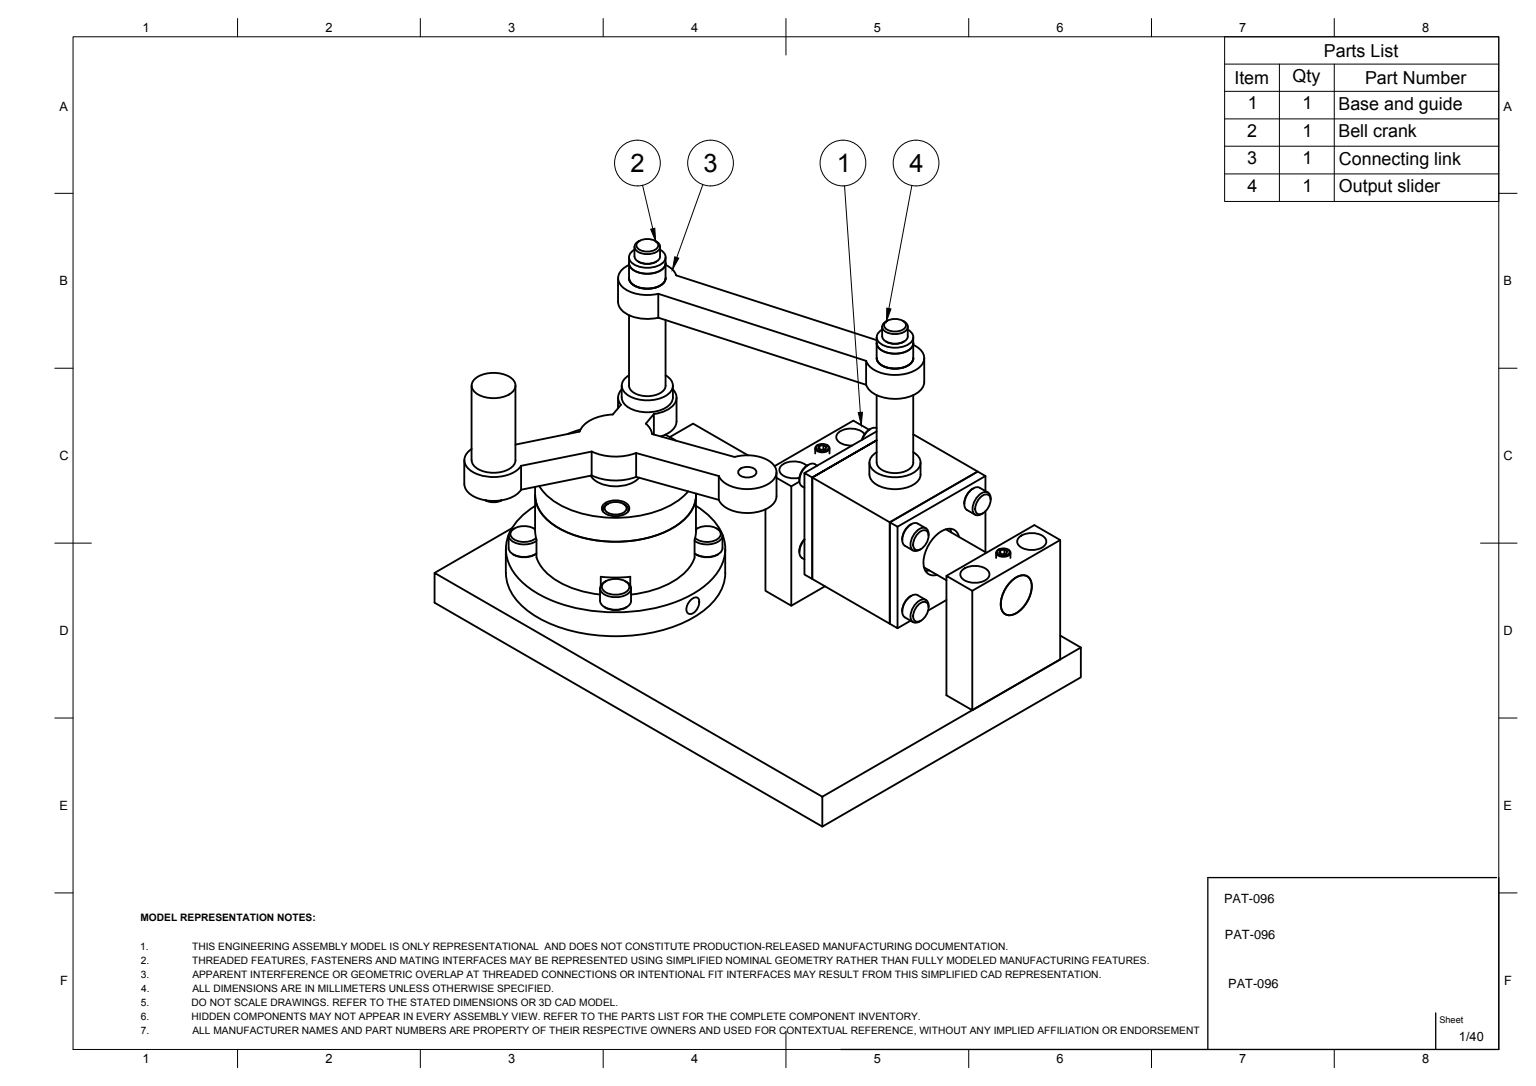
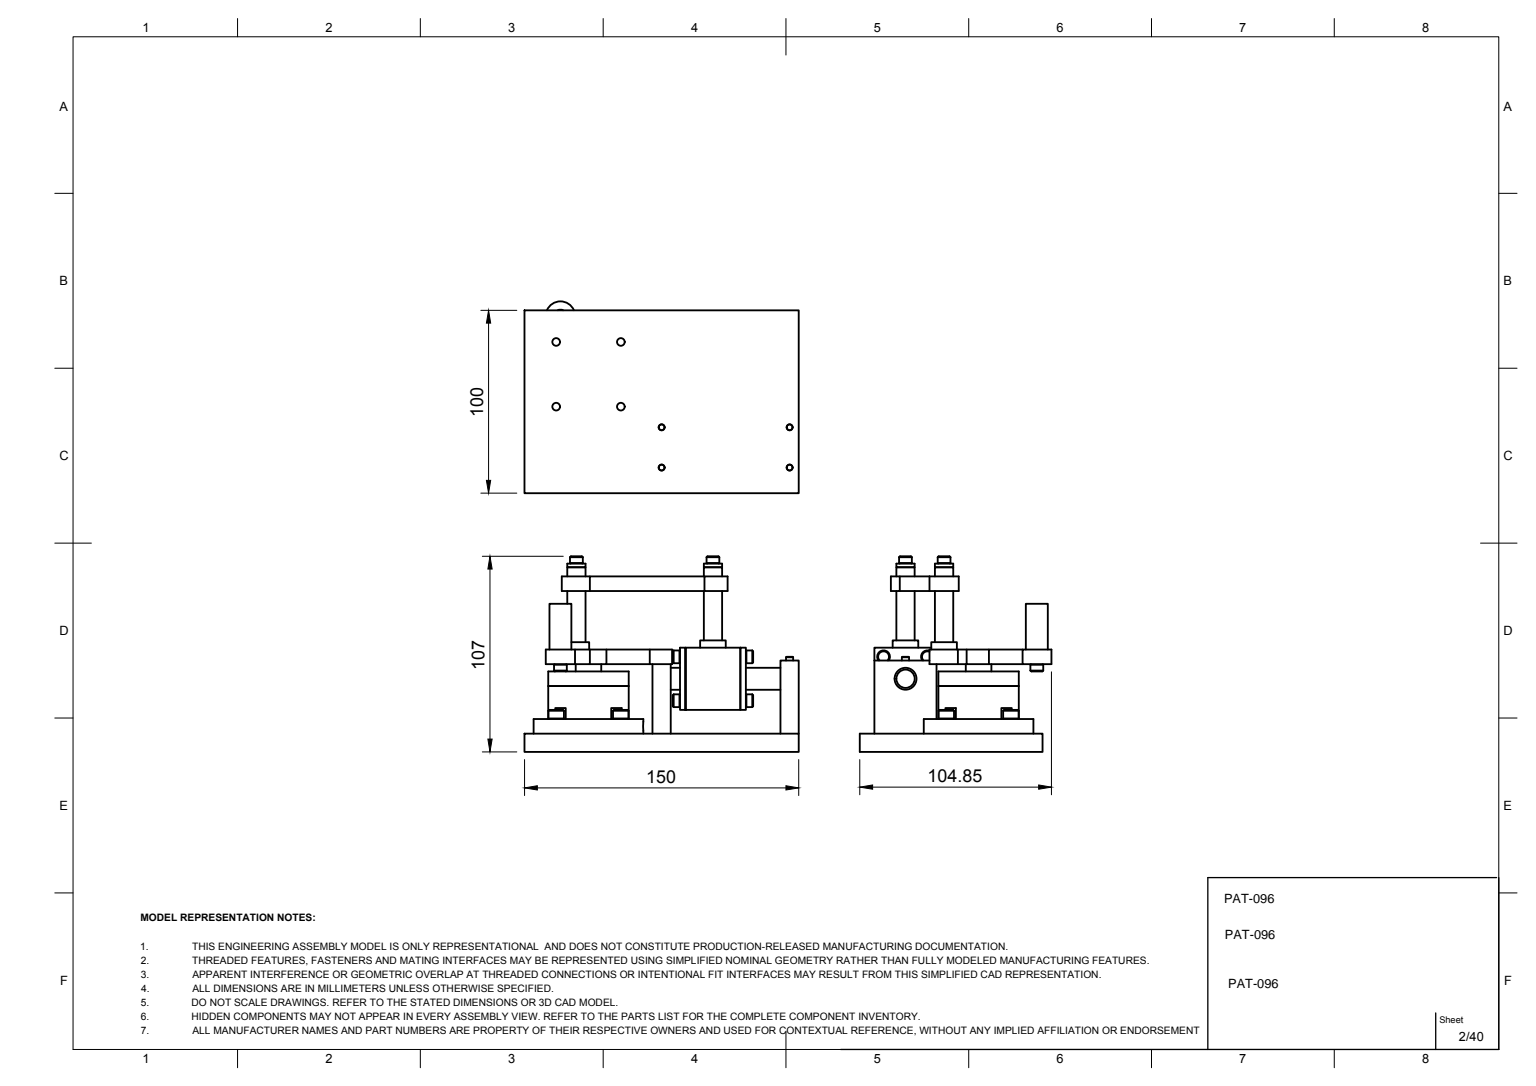
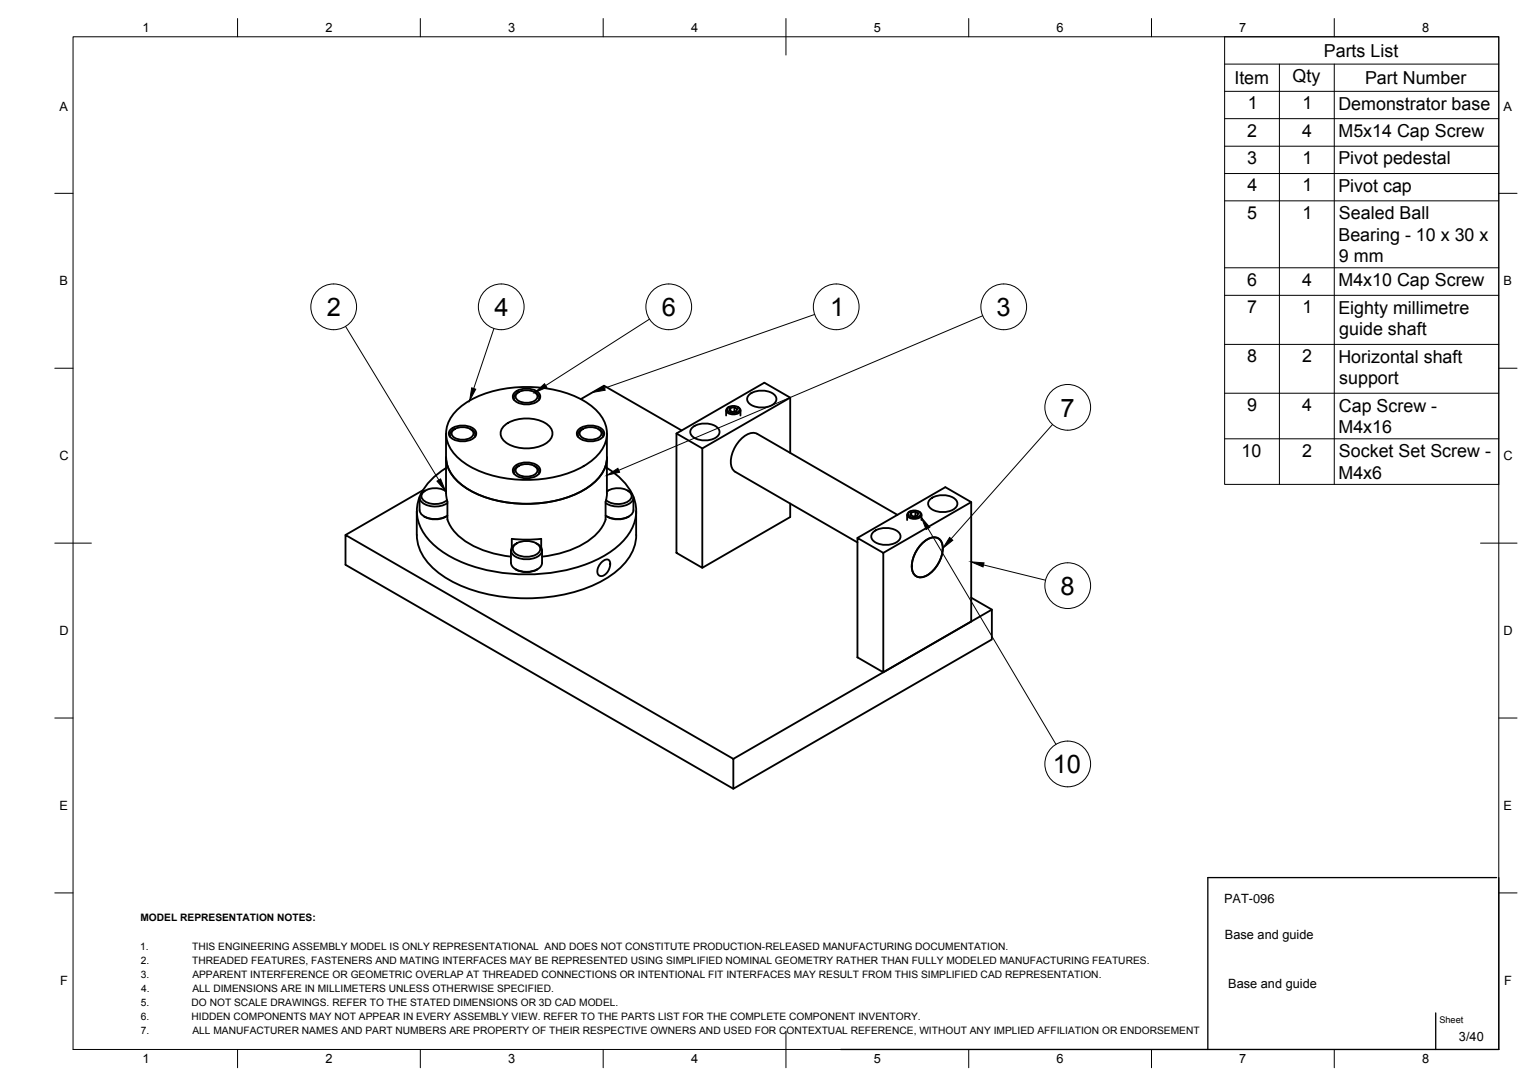
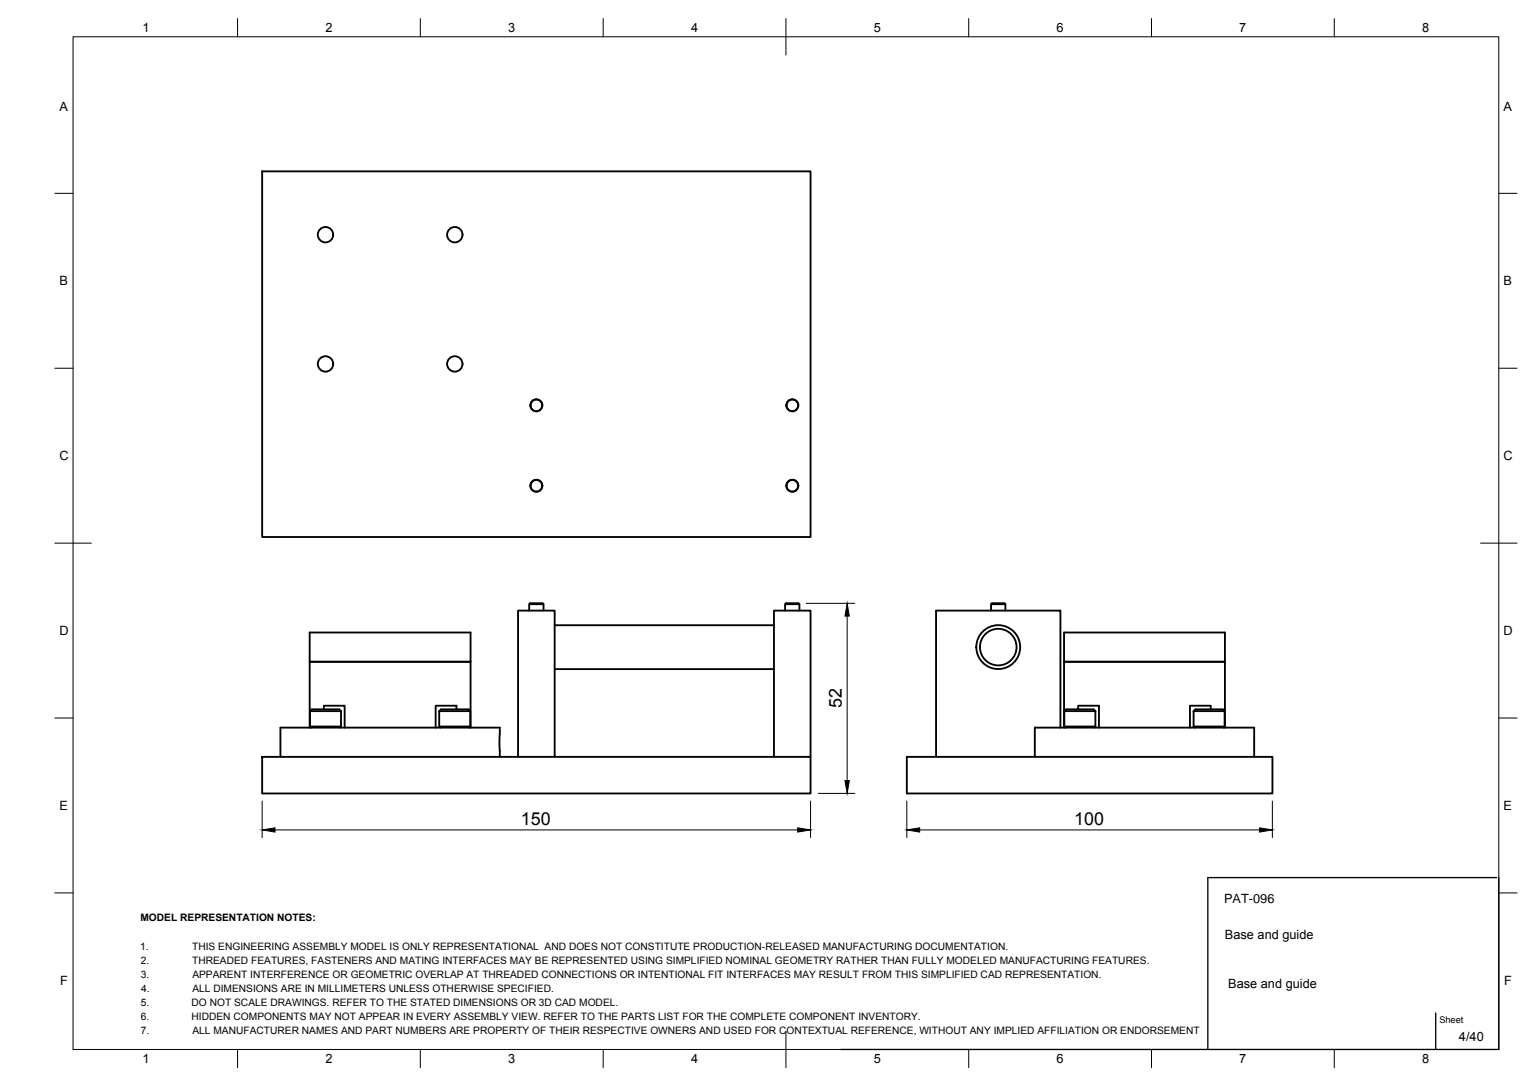
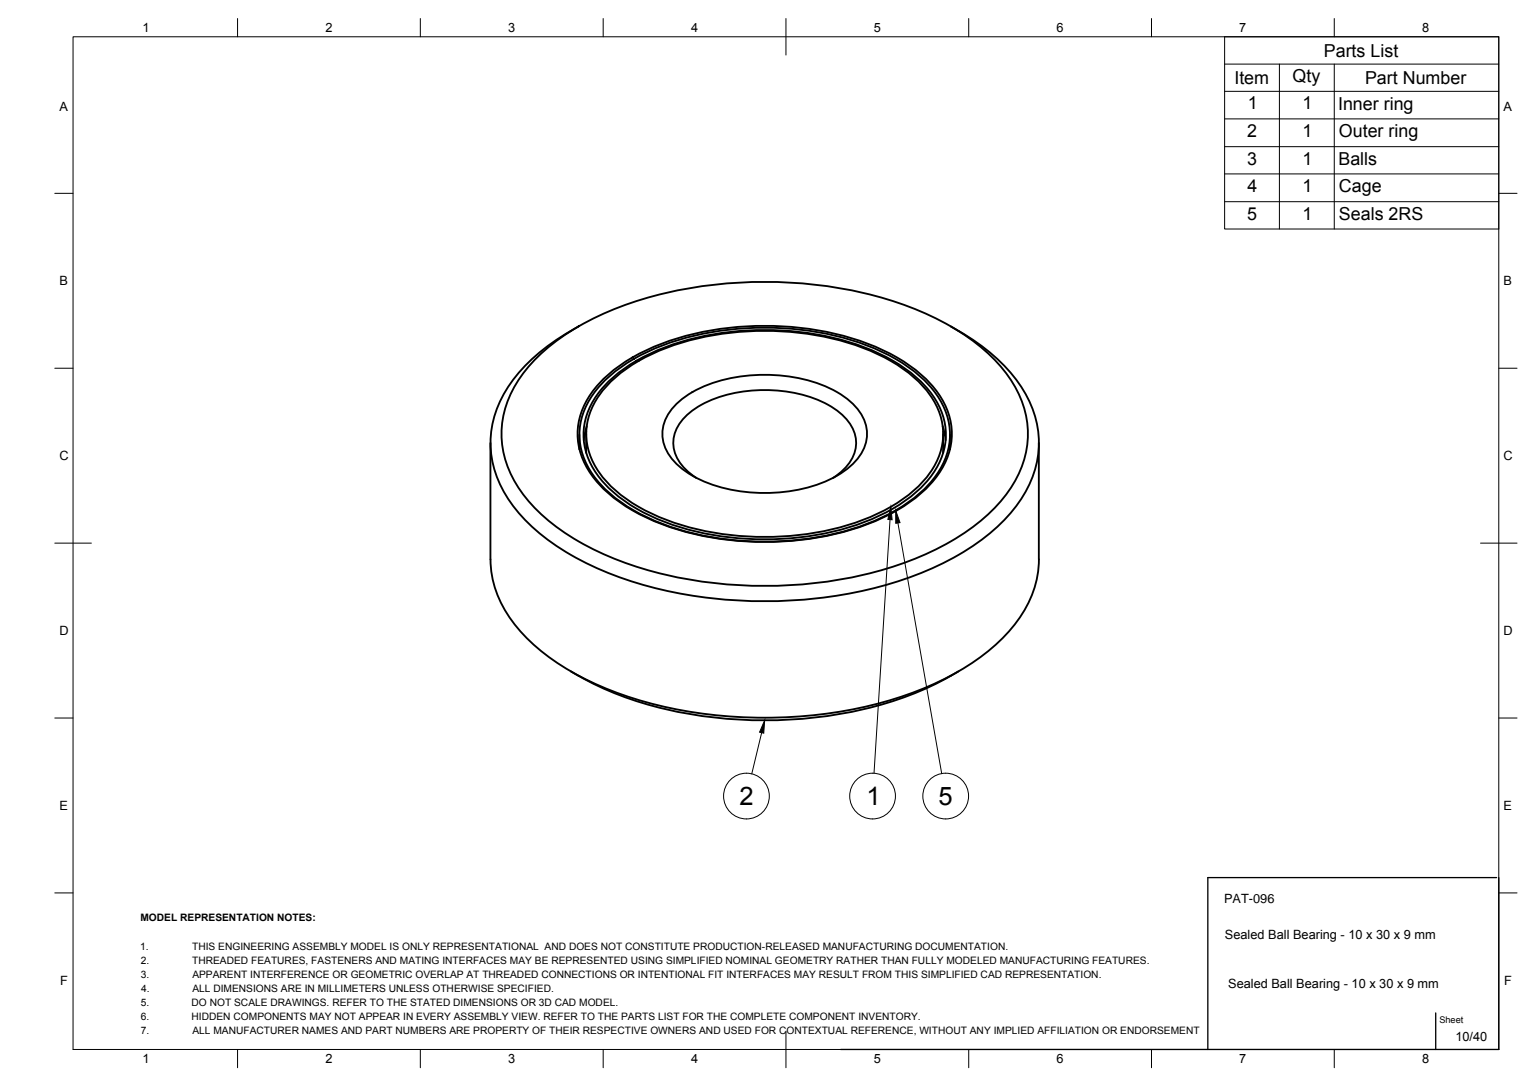
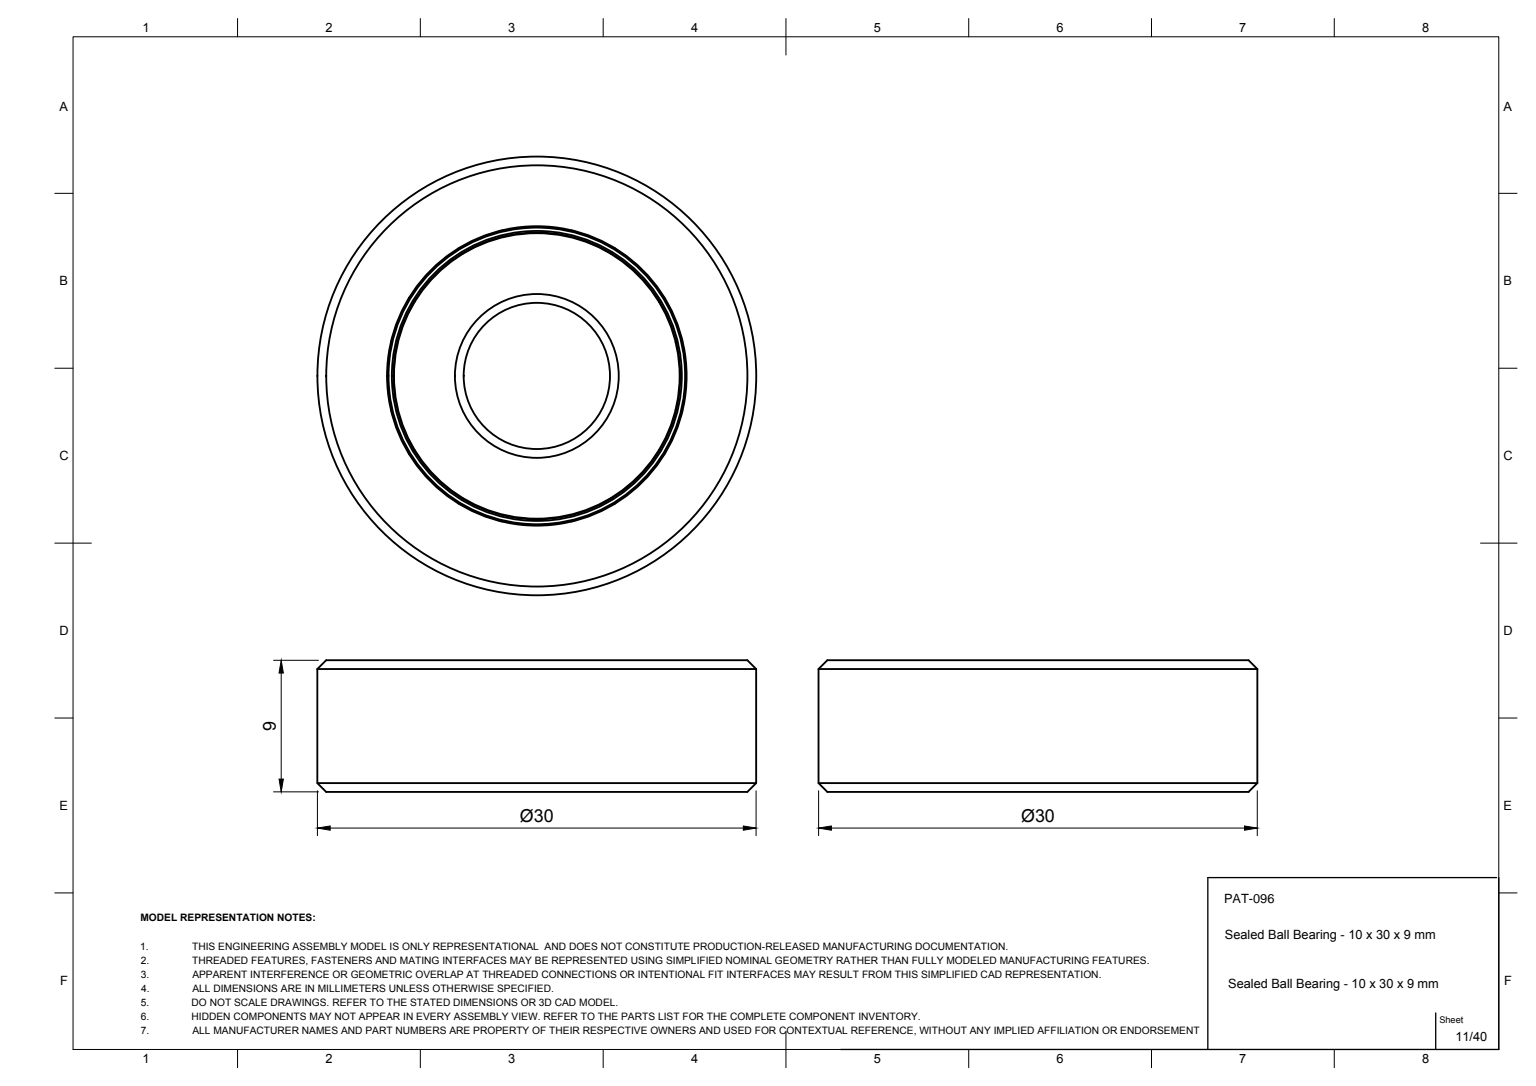
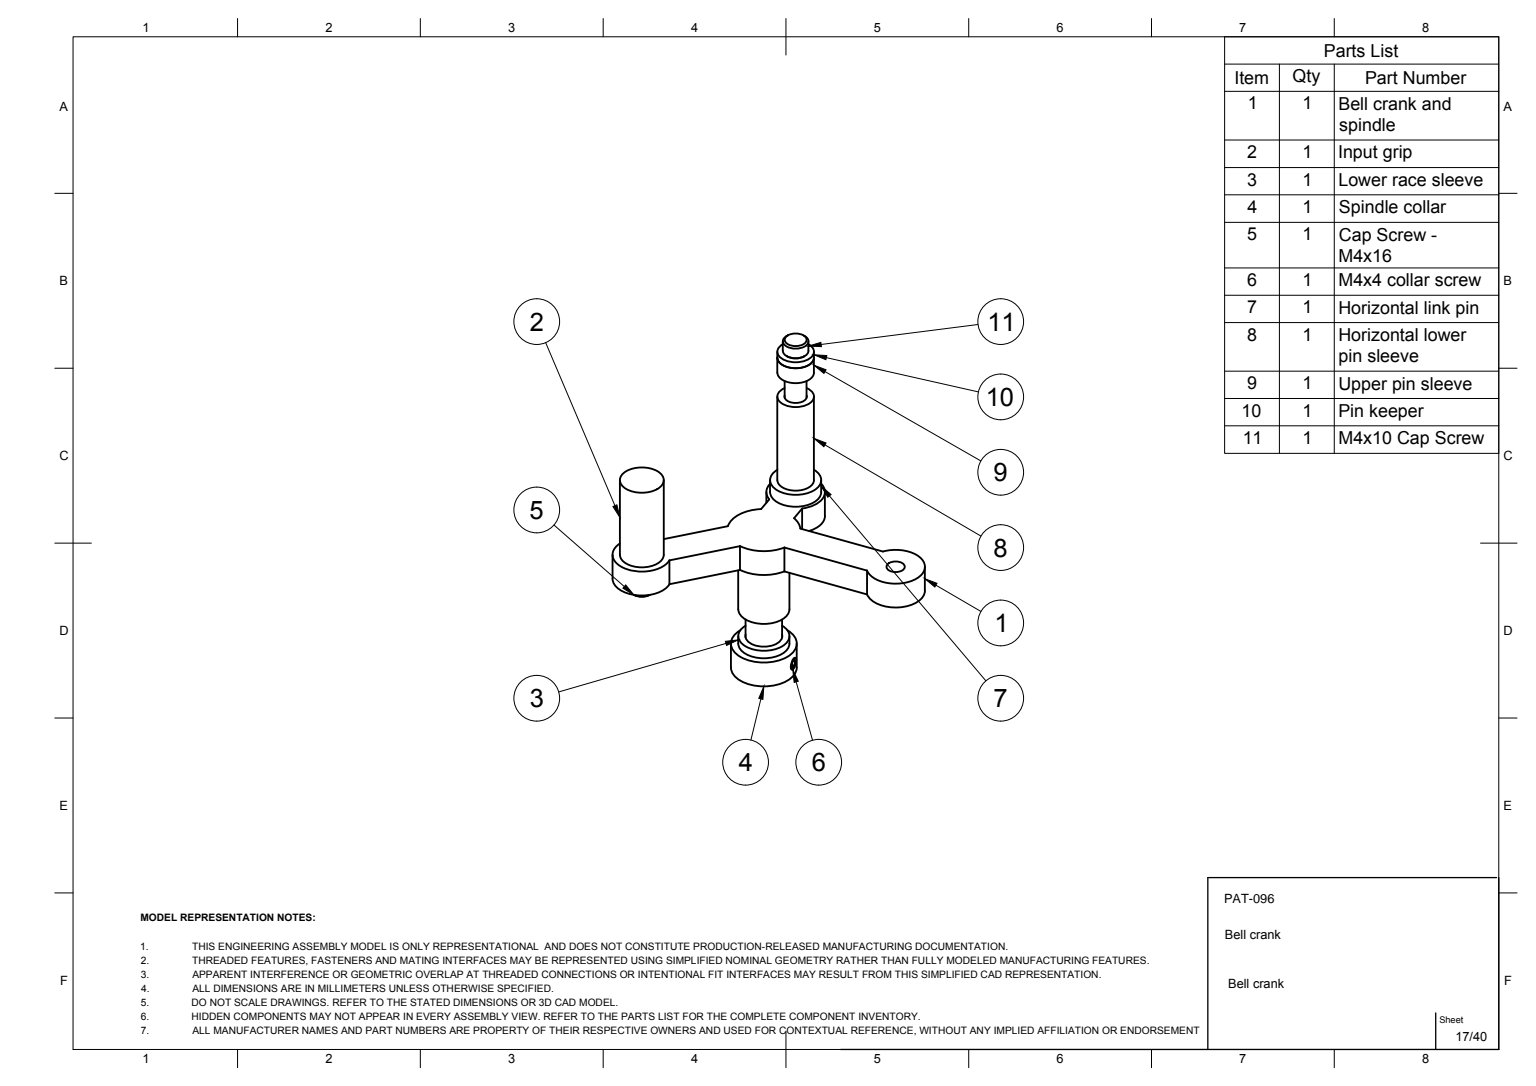
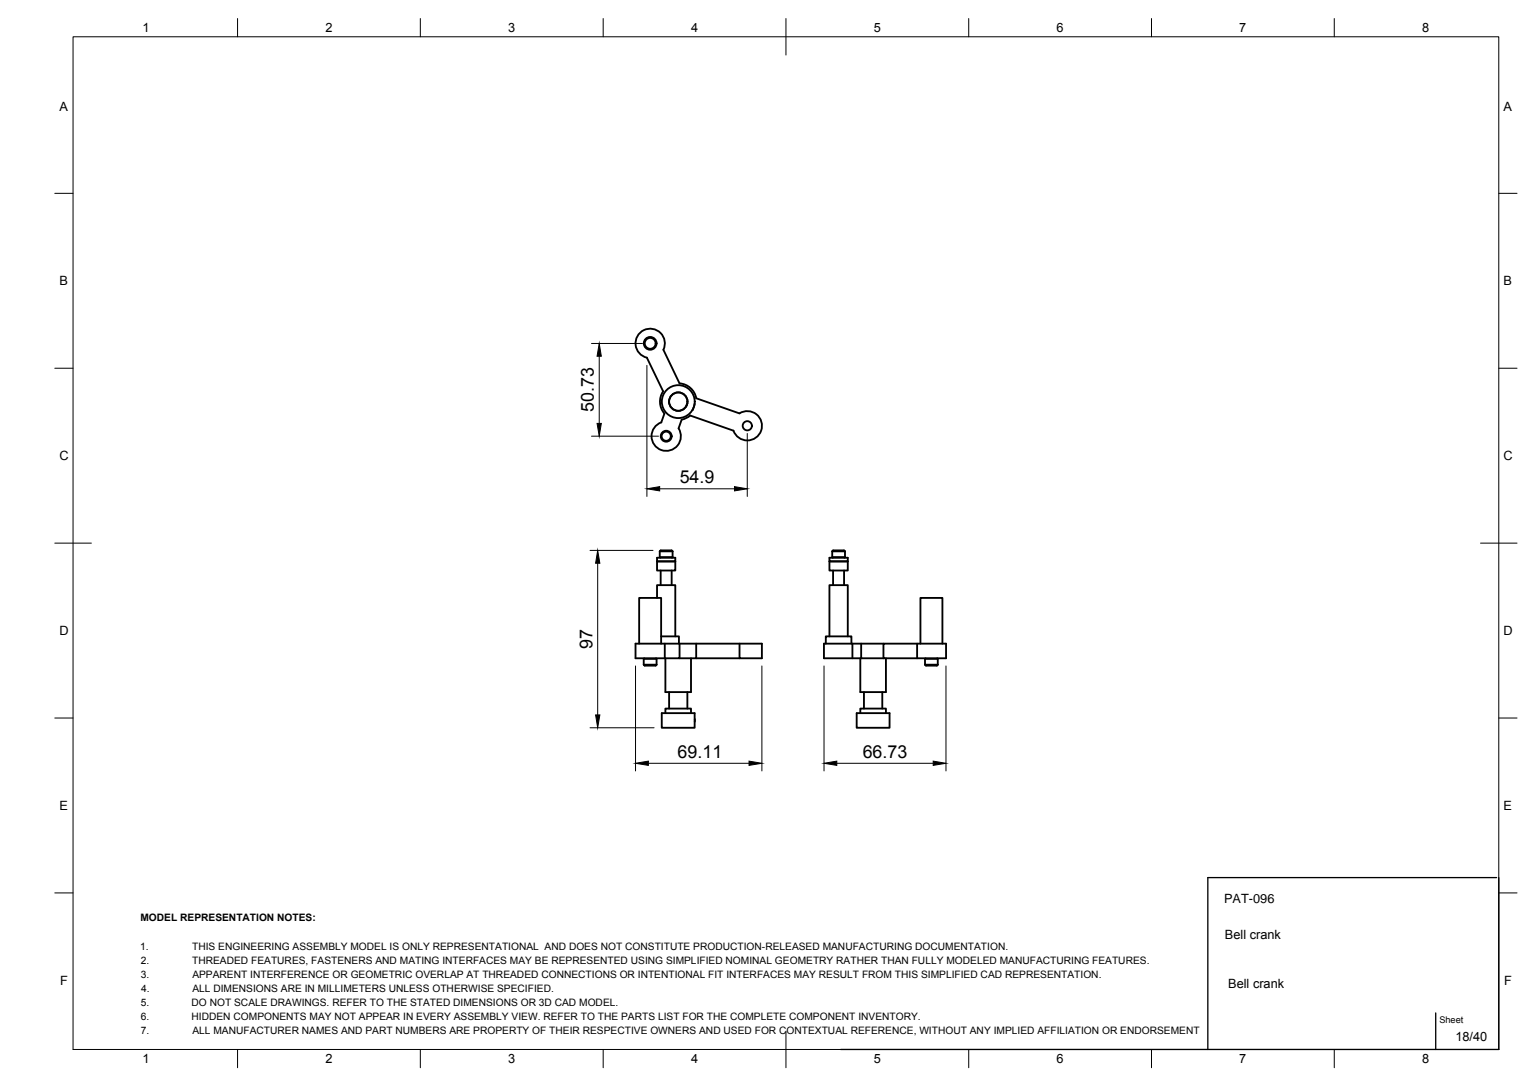
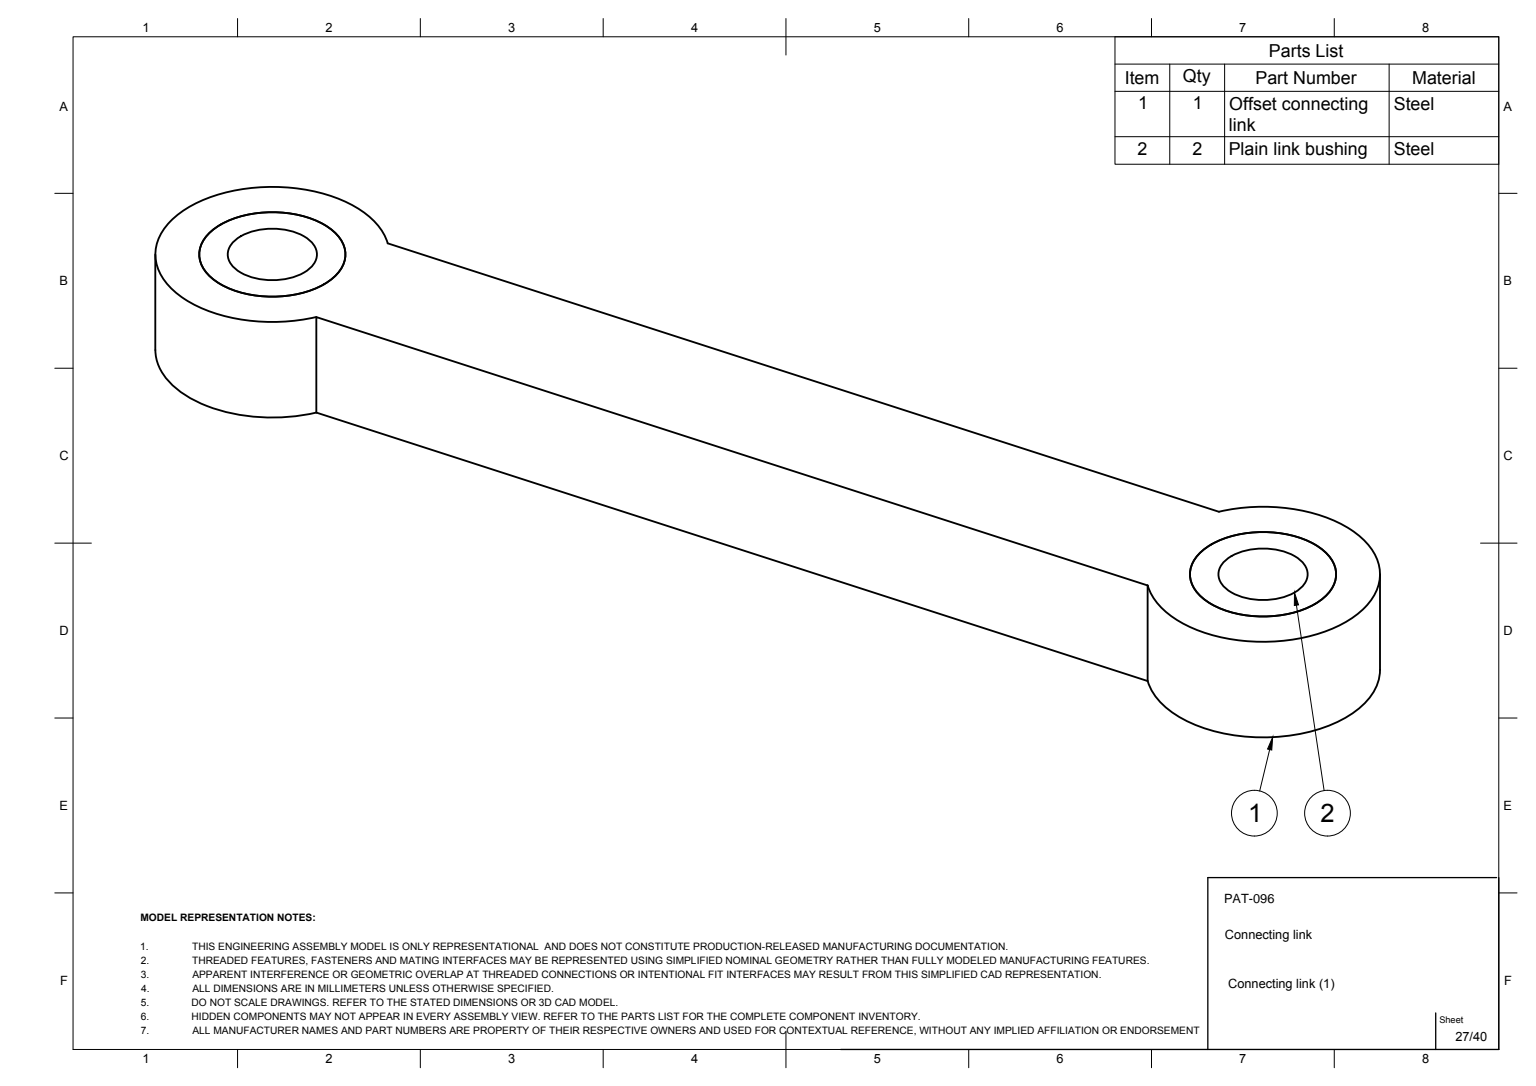
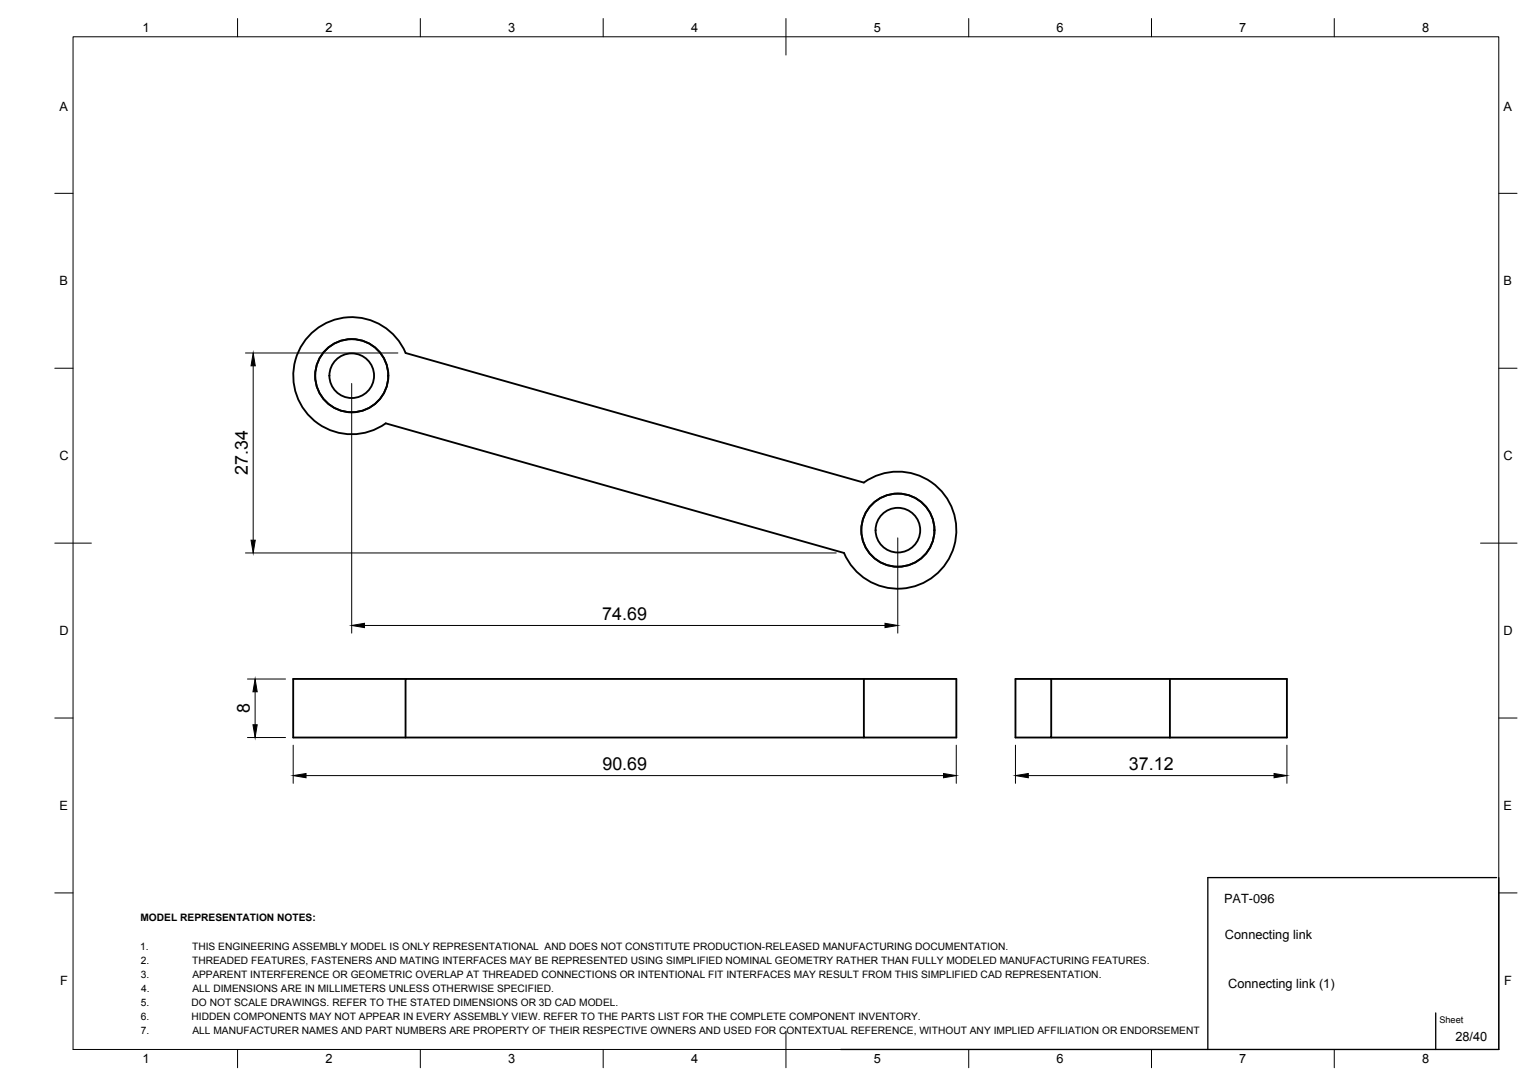
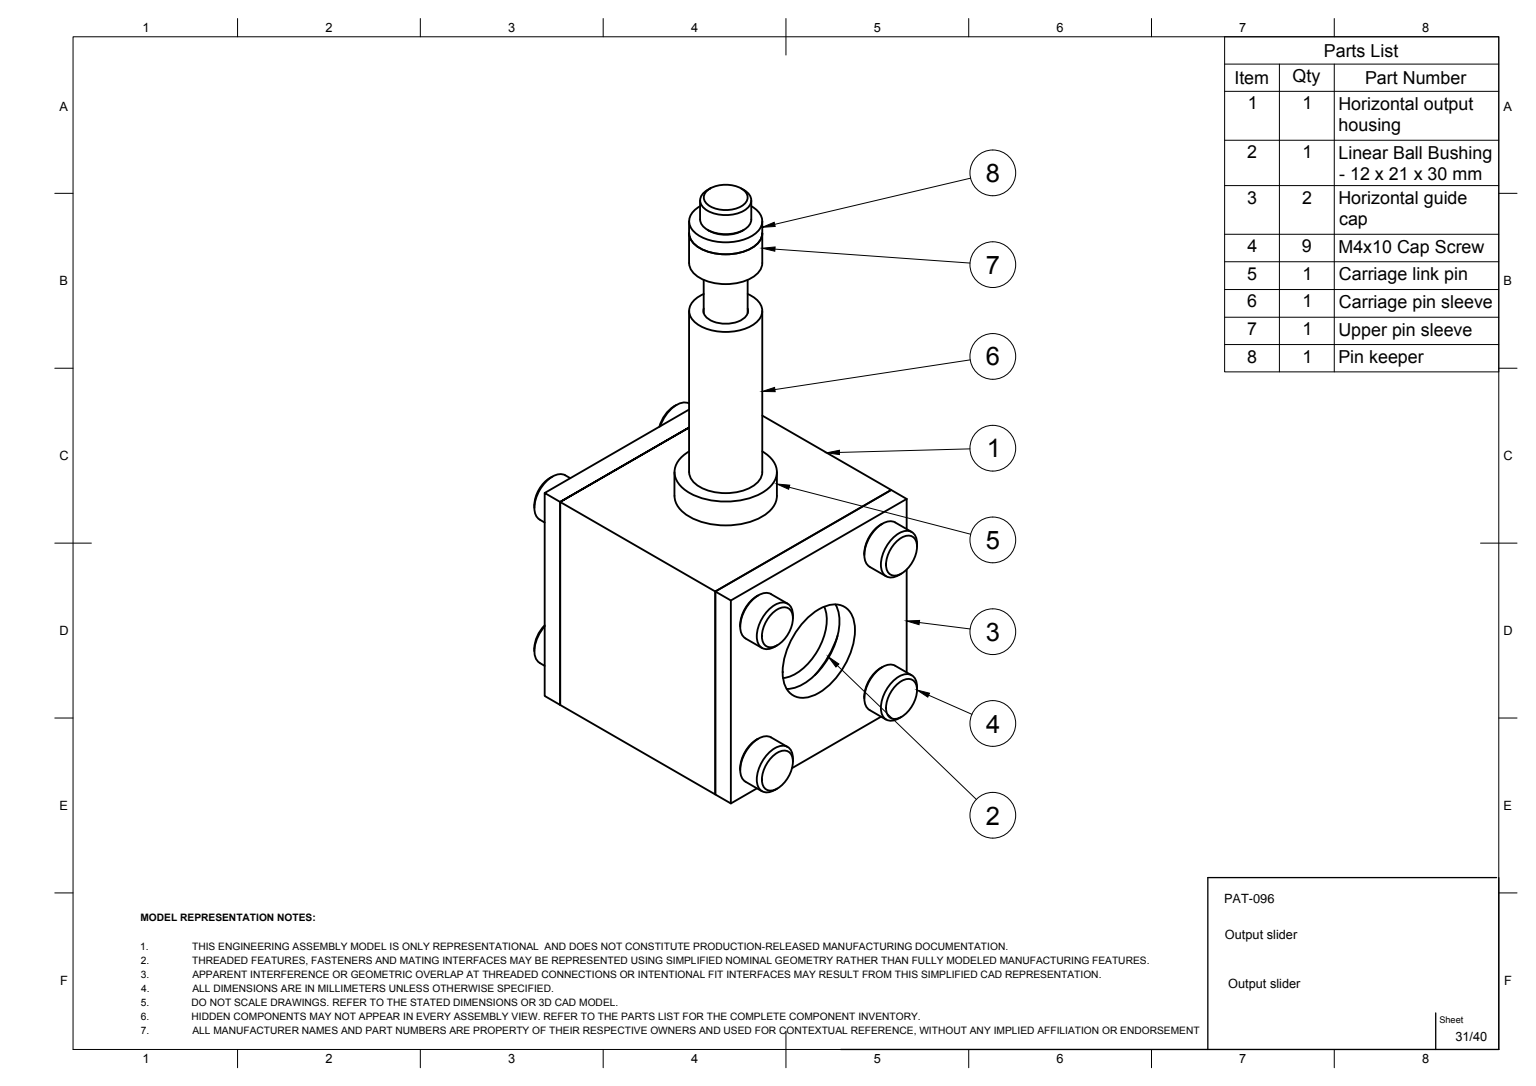
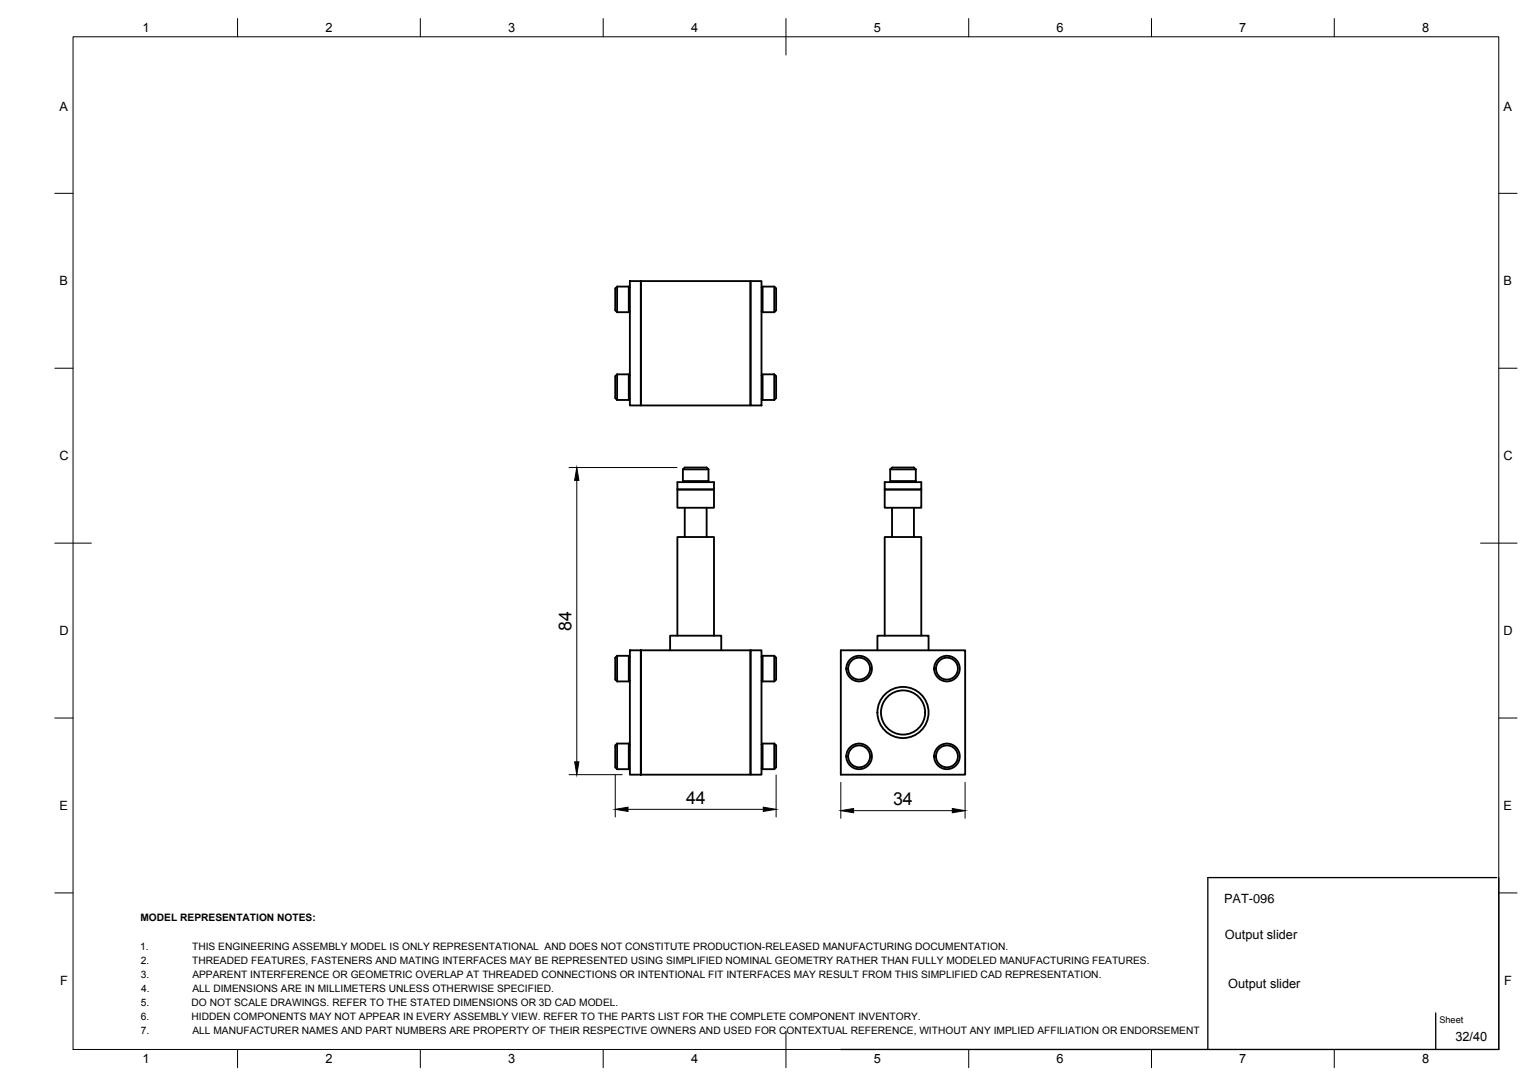
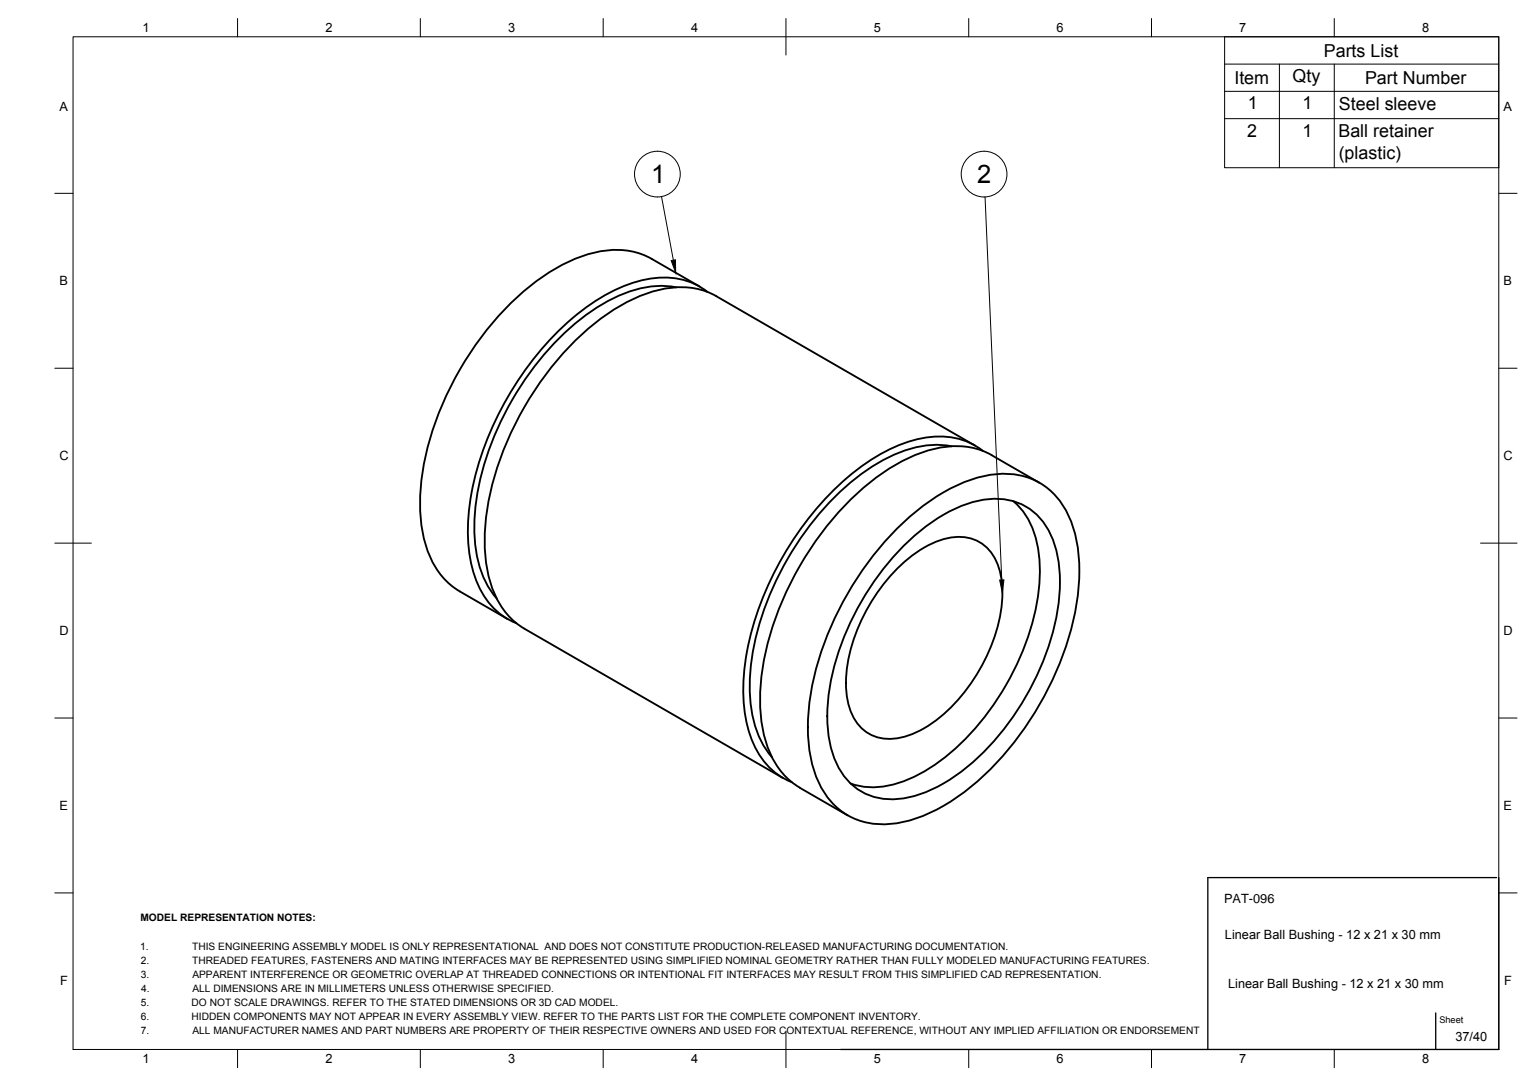
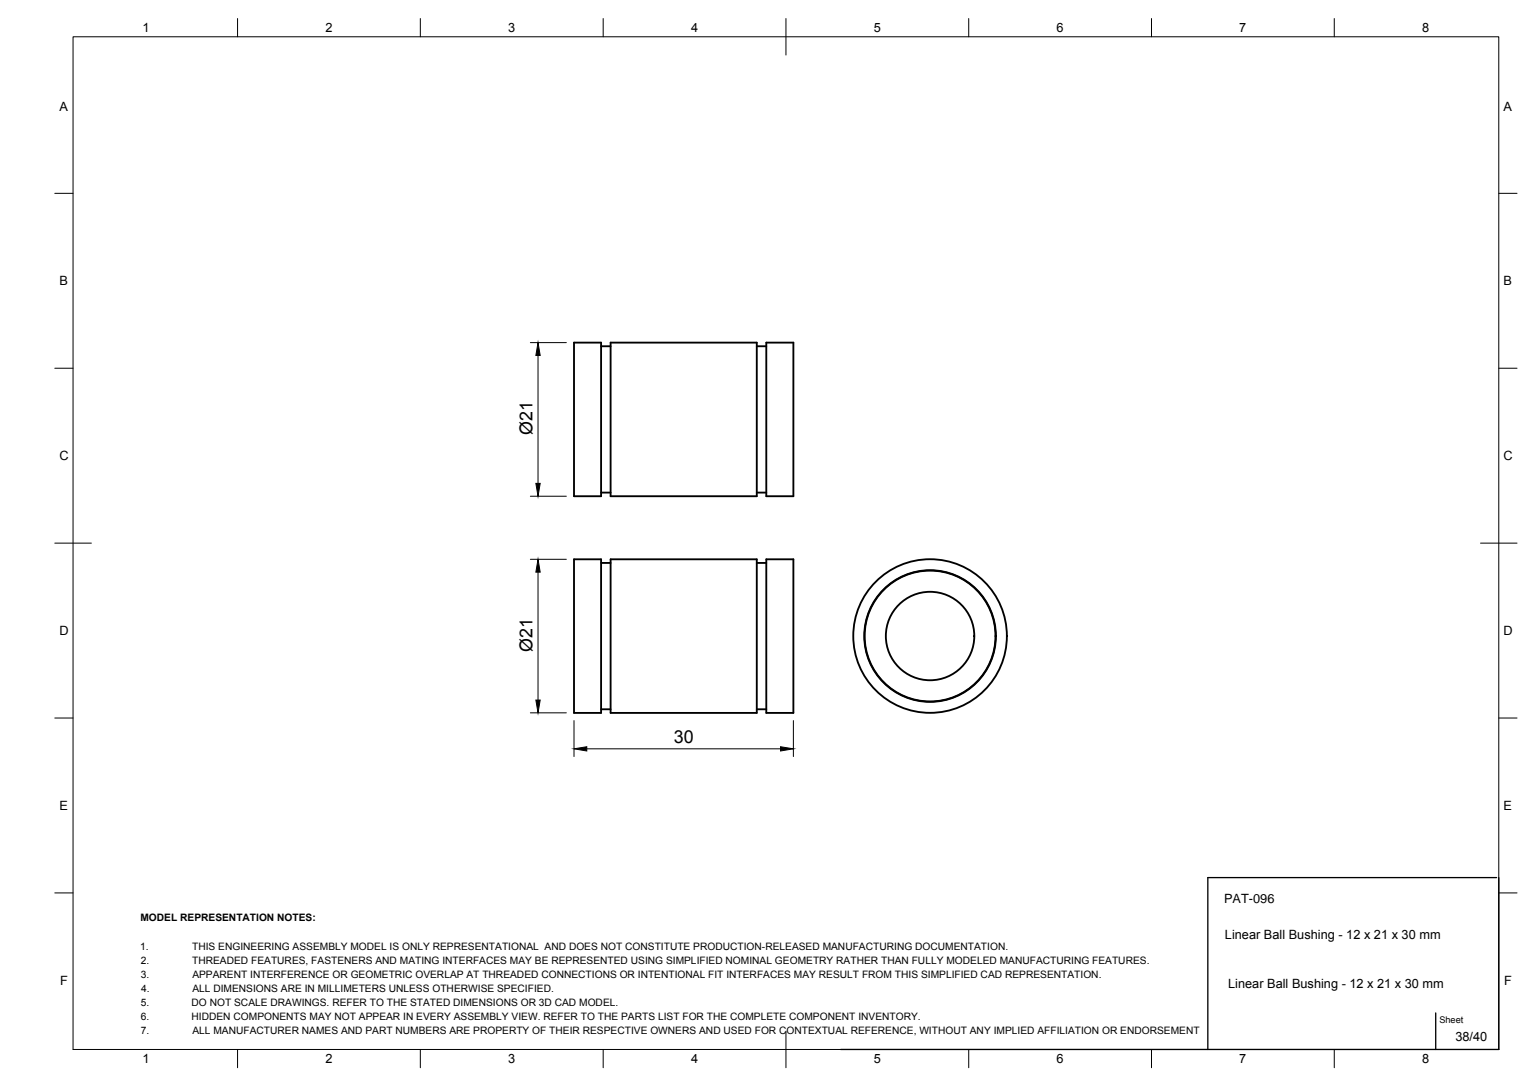
ISO-10303-21;
HEADER;
/* Generated by software containing ST-Developer
 * from STEP Tools, Inc. (www.steptools.com) 
 */

FILE_DESCRIPTION(
/* description */ ('PAT-096'),
/* implementation_level */ '2;1');

FILE_NAME(
/* name */ 'PAT-096',
/* time_stamp */ '2026-10-29T17:03:14-07:00',
/* author */ (''),
/* organization */ (''),
/* preprocessor_version */ 'ST-DEVELOPER v20.2',
/* originating_system */ 'Autodesk Translation Framework v15.17.0.0',
/* authorisation */ '');

FILE_SCHEMA (('AUTOMOTIVE_DESIGN { 1 0 10303 214 3 1 1 }'));
ENDSEC;

DATA;
#10=MECHANICAL_DESIGN_GEOMETRIC_PRESENTATION_REPRESENTATION('',(#398,#399,
#400,#401,#402,#403,#404,#405,#406,#407,#408,#409,#410,#411,#412,#413,#414,
#415,#416,#417,#418,#419,#420,#421,#422,#423,#424,#425,#426,#427,#428,#429,
#430,#431,#432,#433,#434,#435,#436),#10650);
#11=ITEM_DEFINED_TRANSFORMATION($,$,#6084,#6212);
#12=ITEM_DEFINED_TRANSFORMATION($,$,#6104,#6213);
#13=ITEM_DEFINED_TRANSFORMATION($,$,#6124,#6214);
#14=ITEM_DEFINED_TRANSFORMATION($,$,#6141,#6215);
#15=ITEM_DEFINED_TRANSFORMATION($,$,#6195,#6216);
#16=ITEM_DEFINED_TRANSFORMATION($,$,#6419,#6445);
#17=ITEM_DEFINED_TRANSFORMATION($,$,#6436,#6446);
#18=ITEM_DEFINED_TRANSFORMATION($,$,#6436,#6447);
#19=ITEM_DEFINED_TRANSFORMATION($,$,#6503,#6552);
#20=ITEM_DEFINED_TRANSFORMATION($,$,#6535,#6553);
#21=ITEM_DEFINED_TRANSFORMATION($,$,#5917,#6618);
#22=ITEM_DEFINED_TRANSFORMATION($,$,#5948,#6619);
#23=ITEM_DEFINED_TRANSFORMATION($,$,#5948,#6620);
#24=ITEM_DEFINED_TRANSFORMATION($,$,#5948,#6621);
#25=ITEM_DEFINED_TRANSFORMATION($,$,#5948,#6622);
#26=ITEM_DEFINED_TRANSFORMATION($,$,#5972,#6623);
#27=ITEM_DEFINED_TRANSFORMATION($,$,#6042,#6624);
#28=ITEM_DEFINED_TRANSFORMATION($,$,#6083,#6625);
#29=ITEM_DEFINED_TRANSFORMATION($,$,#6594,#6626);
#30=ITEM_DEFINED_TRANSFORMATION($,$,#6594,#6627);
#31=ITEM_DEFINED_TRANSFORMATION($,$,#6594,#6628);
#32=ITEM_DEFINED_TRANSFORMATION($,$,#6594,#6629);
#33=ITEM_DEFINED_TRANSFORMATION($,$,#6217,#6630);
#34=ITEM_DEFINED_TRANSFORMATION($,$,#6225,#6631);
#35=ITEM_DEFINED_TRANSFORMATION($,$,#6350,#6632);
#36=ITEM_DEFINED_TRANSFORMATION($,$,#6350,#6633);
#37=ITEM_DEFINED_TRANSFORMATION($,$,#6255,#6634);
#38=ITEM_DEFINED_TRANSFORMATION($,$,#6225,#6635);
#39=ITEM_DEFINED_TRANSFORMATION($,$,#6350,#6636);
#40=ITEM_DEFINED_TRANSFORMATION($,$,#6350,#6637);
#41=ITEM_DEFINED_TRANSFORMATION($,$,#6255,#6638);
#42=ITEM_DEFINED_TRANSFORMATION($,$,#6273,#6639);
#43=ITEM_DEFINED_TRANSFORMATION($,$,#6317,#6640);
#44=ITEM_DEFINED_TRANSFORMATION($,$,#6327,#6641);
#45=ITEM_DEFINED_TRANSFORMATION($,$,#6336,#6642);
#46=ITEM_DEFINED_TRANSFORMATION($,$,#6350,#6643);
#47=ITEM_DEFINED_TRANSFORMATION($,$,#6376,#6644);
#48=ITEM_DEFINED_TRANSFORMATION($,$,#6391,#6645);
#49=ITEM_DEFINED_TRANSFORMATION($,$,#6409,#6646);
#50=ITEM_DEFINED_TRANSFORMATION($,$,#6576,#6647);
#51=ITEM_DEFINED_TRANSFORMATION($,$,#6585,#6648);
#52=ITEM_DEFINED_TRANSFORMATION($,$,#6594,#6649);
#53=ITEM_DEFINED_TRANSFORMATION($,$,#6449,#6650);
#54=ITEM_DEFINED_TRANSFORMATION($,$,#6467,#6651);
#55=ITEM_DEFINED_TRANSFORMATION($,$,#6476,#6652);
#56=ITEM_DEFINED_TRANSFORMATION($,$,#6502,#6653);
#57=ITEM_DEFINED_TRANSFORMATION($,$,#6554,#6654);
#58=ITEM_DEFINED_TRANSFORMATION($,$,#6554,#6655);
#59=ITEM_DEFINED_TRANSFORMATION($,$,#6594,#6656);
#60=ITEM_DEFINED_TRANSFORMATION($,$,#6594,#6657);
#61=ITEM_DEFINED_TRANSFORMATION($,$,#6594,#6658);
#62=ITEM_DEFINED_TRANSFORMATION($,$,#6594,#6659);
#63=ITEM_DEFINED_TRANSFORMATION($,$,#6594,#6660);
#64=ITEM_DEFINED_TRANSFORMATION($,$,#6594,#6661);
#65=ITEM_DEFINED_TRANSFORMATION($,$,#6594,#6662);
#66=ITEM_DEFINED_TRANSFORMATION($,$,#6594,#6663);
#67=ITEM_DEFINED_TRANSFORMATION($,$,#6576,#6664);
#68=ITEM_DEFINED_TRANSFORMATION($,$,#6585,#6665);
#69=ITEM_DEFINED_TRANSFORMATION($,$,#6594,#6666);
#70=ITEM_DEFINED_TRANSFORMATION($,$,#5916,#6667);
#71=ITEM_DEFINED_TRANSFORMATION($,$,#6272,#6668);
#72=ITEM_DEFINED_TRANSFORMATION($,$,#6418,#6669);
#73=ITEM_DEFINED_TRANSFORMATION($,$,#6448,#6670);
#74=(
REPRESENTATION_RELATIONSHIP($,$,#10801,#10800)
REPRESENTATION_RELATIONSHIP_WITH_TRANSFORMATION(#11)
SHAPE_REPRESENTATION_RELATIONSHIP()
);
#75=(
REPRESENTATION_RELATIONSHIP($,$,#10802,#10800)
REPRESENTATION_RELATIONSHIP_WITH_TRANSFORMATION(#12)
SHAPE_REPRESENTATION_RELATIONSHIP()
);
#76=(
REPRESENTATION_RELATIONSHIP($,$,#10803,#10800)
REPRESENTATION_RELATIONSHIP_WITH_TRANSFORMATION(#13)
SHAPE_REPRESENTATION_RELATIONSHIP()
);
#77=(
REPRESENTATION_RELATIONSHIP($,$,#10804,#10800)
REPRESENTATION_RELATIONSHIP_WITH_TRANSFORMATION(#14)
SHAPE_REPRESENTATION_RELATIONSHIP()
);
#78=(
REPRESENTATION_RELATIONSHIP($,$,#10805,#10800)
REPRESENTATION_RELATIONSHIP_WITH_TRANSFORMATION(#15)
SHAPE_REPRESENTATION_RELATIONSHIP()
);
#79=(
REPRESENTATION_RELATIONSHIP($,$,#10819,#10818)
REPRESENTATION_RELATIONSHIP_WITH_TRANSFORMATION(#16)
SHAPE_REPRESENTATION_RELATIONSHIP()
);
#80=(
REPRESENTATION_RELATIONSHIP($,$,#10820,#10818)
REPRESENTATION_RELATIONSHIP_WITH_TRANSFORMATION(#17)
SHAPE_REPRESENTATION_RELATIONSHIP()
);
#81=(
REPRESENTATION_RELATIONSHIP($,$,#10820,#10818)
REPRESENTATION_RELATIONSHIP_WITH_TRANSFORMATION(#18)
SHAPE_REPRESENTATION_RELATIONSHIP()
);
#82=(
REPRESENTATION_RELATIONSHIP($,$,#10826,#10825)
REPRESENTATION_RELATIONSHIP_WITH_TRANSFORMATION(#19)
SHAPE_REPRESENTATION_RELATIONSHIP()
);
#83=(
REPRESENTATION_RELATIONSHIP($,$,#10827,#10825)
REPRESENTATION_RELATIONSHIP_WITH_TRANSFORMATION(#20)
SHAPE_REPRESENTATION_RELATIONSHIP()
);
#84=(
REPRESENTATION_RELATIONSHIP($,$,#10796,#10795)
REPRESENTATION_RELATIONSHIP_WITH_TRANSFORMATION(#21)
SHAPE_REPRESENTATION_RELATIONSHIP()
);
#85=(
REPRESENTATION_RELATIONSHIP($,$,#10797,#10795)
REPRESENTATION_RELATIONSHIP_WITH_TRANSFORMATION(#22)
SHAPE_REPRESENTATION_RELATIONSHIP()
);
#86=(
REPRESENTATION_RELATIONSHIP($,$,#10797,#10795)
REPRESENTATION_RELATIONSHIP_WITH_TRANSFORMATION(#23)
SHAPE_REPRESENTATION_RELATIONSHIP()
);
#87=(
REPRESENTATION_RELATIONSHIP($,$,#10797,#10795)
REPRESENTATION_RELATIONSHIP_WITH_TRANSFORMATION(#24)
SHAPE_REPRESENTATION_RELATIONSHIP()
);
#88=(
REPRESENTATION_RELATIONSHIP($,$,#10797,#10795)
REPRESENTATION_RELATIONSHIP_WITH_TRANSFORMATION(#25)
SHAPE_REPRESENTATION_RELATIONSHIP()
);
#89=(
REPRESENTATION_RELATIONSHIP($,$,#10798,#10795)
REPRESENTATION_RELATIONSHIP_WITH_TRANSFORMATION(#26)
SHAPE_REPRESENTATION_RELATIONSHIP()
);
#90=(
REPRESENTATION_RELATIONSHIP($,$,#10799,#10795)
REPRESENTATION_RELATIONSHIP_WITH_TRANSFORMATION(#27)
SHAPE_REPRESENTATION_RELATIONSHIP()
);
#91=(
REPRESENTATION_RELATIONSHIP($,$,#10800,#10795)
REPRESENTATION_RELATIONSHIP_WITH_TRANSFORMATION(#28)
SHAPE_REPRESENTATION_RELATIONSHIP()
);
#92=(
REPRESENTATION_RELATIONSHIP($,$,#10831,#10795)
REPRESENTATION_RELATIONSHIP_WITH_TRANSFORMATION(#29)
SHAPE_REPRESENTATION_RELATIONSHIP()
);
#93=(
REPRESENTATION_RELATIONSHIP($,$,#10831,#10795)
REPRESENTATION_RELATIONSHIP_WITH_TRANSFORMATION(#30)
SHAPE_REPRESENTATION_RELATIONSHIP()
);
#94=(
REPRESENTATION_RELATIONSHIP($,$,#10831,#10795)
REPRESENTATION_RELATIONSHIP_WITH_TRANSFORMATION(#31)
SHAPE_REPRESENTATION_RELATIONSHIP()
);
#95=(
REPRESENTATION_RELATIONSHIP($,$,#10831,#10795)
REPRESENTATION_RELATIONSHIP_WITH_TRANSFORMATION(#32)
SHAPE_REPRESENTATION_RELATIONSHIP()
);
#96=(
REPRESENTATION_RELATIONSHIP($,$,#10806,#10795)
REPRESENTATION_RELATIONSHIP_WITH_TRANSFORMATION(#33)
SHAPE_REPRESENTATION_RELATIONSHIP()
);
#97=(
REPRESENTATION_RELATIONSHIP($,$,#10807,#10795)
REPRESENTATION_RELATIONSHIP_WITH_TRANSFORMATION(#34)
SHAPE_REPRESENTATION_RELATIONSHIP()
);
#98=(
REPRESENTATION_RELATIONSHIP($,$,#10814,#10795)
REPRESENTATION_RELATIONSHIP_WITH_TRANSFORMATION(#35)
SHAPE_REPRESENTATION_RELATIONSHIP()
);
#99=(
REPRESENTATION_RELATIONSHIP($,$,#10814,#10795)
REPRESENTATION_RELATIONSHIP_WITH_TRANSFORMATION(#36)
SHAPE_REPRESENTATION_RELATIONSHIP()
);
#100=(
REPRESENTATION_RELATIONSHIP($,$,#10808,#10795)
REPRESENTATION_RELATIONSHIP_WITH_TRANSFORMATION(#37)
SHAPE_REPRESENTATION_RELATIONSHIP()
);
#101=(
REPRESENTATION_RELATIONSHIP($,$,#10807,#10795)
REPRESENTATION_RELATIONSHIP_WITH_TRANSFORMATION(#38)
SHAPE_REPRESENTATION_RELATIONSHIP()
);
#102=(
REPRESENTATION_RELATIONSHIP($,$,#10814,#10795)
REPRESENTATION_RELATIONSHIP_WITH_TRANSFORMATION(#39)
SHAPE_REPRESENTATION_RELATIONSHIP()
);
#103=(
REPRESENTATION_RELATIONSHIP($,$,#10814,#10795)
REPRESENTATION_RELATIONSHIP_WITH_TRANSFORMATION(#40)
SHAPE_REPRESENTATION_RELATIONSHIP()
);
#104=(
REPRESENTATION_RELATIONSHIP($,$,#10808,#10795)
REPRESENTATION_RELATIONSHIP_WITH_TRANSFORMATION(#41)
SHAPE_REPRESENTATION_RELATIONSHIP()
);
#105=(
REPRESENTATION_RELATIONSHIP($,$,#10810,#10809)
REPRESENTATION_RELATIONSHIP_WITH_TRANSFORMATION(#42)
SHAPE_REPRESENTATION_RELATIONSHIP()
);
#106=(
REPRESENTATION_RELATIONSHIP($,$,#10811,#10809)
REPRESENTATION_RELATIONSHIP_WITH_TRANSFORMATION(#43)
SHAPE_REPRESENTATION_RELATIONSHIP()
);
#107=(
REPRESENTATION_RELATIONSHIP($,$,#10812,#10809)
REPRESENTATION_RELATIONSHIP_WITH_TRANSFORMATION(#44)
SHAPE_REPRESENTATION_RELATIONSHIP()
);
#108=(
REPRESENTATION_RELATIONSHIP($,$,#10813,#10809)
REPRESENTATION_RELATIONSHIP_WITH_TRANSFORMATION(#45)
SHAPE_REPRESENTATION_RELATIONSHIP()
);
#109=(
REPRESENTATION_RELATIONSHIP($,$,#10814,#10809)
REPRESENTATION_RELATIONSHIP_WITH_TRANSFORMATION(#46)
SHAPE_REPRESENTATION_RELATIONSHIP()
);
#110=(
REPRESENTATION_RELATIONSHIP($,$,#10815,#10809)
REPRESENTATION_RELATIONSHIP_WITH_TRANSFORMATION(#47)
SHAPE_REPRESENTATION_RELATIONSHIP()
);
#111=(
REPRESENTATION_RELATIONSHIP($,$,#10816,#10809)
REPRESENTATION_RELATIONSHIP_WITH_TRANSFORMATION(#48)
SHAPE_REPRESENTATION_RELATIONSHIP()
);
#112=(
REPRESENTATION_RELATIONSHIP($,$,#10817,#10809)
REPRESENTATION_RELATIONSHIP_WITH_TRANSFORMATION(#49)
SHAPE_REPRESENTATION_RELATIONSHIP()
);
#113=(
REPRESENTATION_RELATIONSHIP($,$,#10829,#10809)
REPRESENTATION_RELATIONSHIP_WITH_TRANSFORMATION(#50)
SHAPE_REPRESENTATION_RELATIONSHIP()
);
#114=(
REPRESENTATION_RELATIONSHIP($,$,#10830,#10809)
REPRESENTATION_RELATIONSHIP_WITH_TRANSFORMATION(#51)
SHAPE_REPRESENTATION_RELATIONSHIP()
);
#115=(
REPRESENTATION_RELATIONSHIP($,$,#10831,#10809)
REPRESENTATION_RELATIONSHIP_WITH_TRANSFORMATION(#52)
SHAPE_REPRESENTATION_RELATIONSHIP()
);
#116=(
REPRESENTATION_RELATIONSHIP($,$,#10822,#10821)
REPRESENTATION_RELATIONSHIP_WITH_TRANSFORMATION(#53)
SHAPE_REPRESENTATION_RELATIONSHIP()
);
#117=(
REPRESENTATION_RELATIONSHIP($,$,#10823,#10821)
REPRESENTATION_RELATIONSHIP_WITH_TRANSFORMATION(#54)
SHAPE_REPRESENTATION_RELATIONSHIP()
);
#118=(
REPRESENTATION_RELATIONSHIP($,$,#10824,#10821)
REPRESENTATION_RELATIONSHIP_WITH_TRANSFORMATION(#55)
SHAPE_REPRESENTATION_RELATIONSHIP()
);
#119=(
REPRESENTATION_RELATIONSHIP($,$,#10825,#10821)
REPRESENTATION_RELATIONSHIP_WITH_TRANSFORMATION(#56)
SHAPE_REPRESENTATION_RELATIONSHIP()
);
#120=(
REPRESENTATION_RELATIONSHIP($,$,#10828,#10821)
REPRESENTATION_RELATIONSHIP_WITH_TRANSFORMATION(#57)
SHAPE_REPRESENTATION_RELATIONSHIP()
);
#121=(
REPRESENTATION_RELATIONSHIP($,$,#10828,#10821)
REPRESENTATION_RELATIONSHIP_WITH_TRANSFORMATION(#58)
SHAPE_REPRESENTATION_RELATIONSHIP()
);
#122=(
REPRESENTATION_RELATIONSHIP($,$,#10831,#10821)
REPRESENTATION_RELATIONSHIP_WITH_TRANSFORMATION(#59)
SHAPE_REPRESENTATION_RELATIONSHIP()
);
#123=(
REPRESENTATION_RELATIONSHIP($,$,#10831,#10821)
REPRESENTATION_RELATIONSHIP_WITH_TRANSFORMATION(#60)
SHAPE_REPRESENTATION_RELATIONSHIP()
);
#124=(
REPRESENTATION_RELATIONSHIP($,$,#10831,#10821)
REPRESENTATION_RELATIONSHIP_WITH_TRANSFORMATION(#61)
SHAPE_REPRESENTATION_RELATIONSHIP()
);
#125=(
REPRESENTATION_RELATIONSHIP($,$,#10831,#10821)
REPRESENTATION_RELATIONSHIP_WITH_TRANSFORMATION(#62)
SHAPE_REPRESENTATION_RELATIONSHIP()
);
#126=(
REPRESENTATION_RELATIONSHIP($,$,#10831,#10821)
REPRESENTATION_RELATIONSHIP_WITH_TRANSFORMATION(#63)
SHAPE_REPRESENTATION_RELATIONSHIP()
);
#127=(
REPRESENTATION_RELATIONSHIP($,$,#10831,#10821)
REPRESENTATION_RELATIONSHIP_WITH_TRANSFORMATION(#64)
SHAPE_REPRESENTATION_RELATIONSHIP()
);
#128=(
REPRESENTATION_RELATIONSHIP($,$,#10831,#10821)
REPRESENTATION_RELATIONSHIP_WITH_TRANSFORMATION(#65)
SHAPE_REPRESENTATION_RELATIONSHIP()
);
#129=(
REPRESENTATION_RELATIONSHIP($,$,#10831,#10821)
REPRESENTATION_RELATIONSHIP_WITH_TRANSFORMATION(#66)
SHAPE_REPRESENTATION_RELATIONSHIP()
);
#130=(
REPRESENTATION_RELATIONSHIP($,$,#10829,#10821)
REPRESENTATION_RELATIONSHIP_WITH_TRANSFORMATION(#67)
SHAPE_REPRESENTATION_RELATIONSHIP()
);
#131=(
REPRESENTATION_RELATIONSHIP($,$,#10830,#10821)
REPRESENTATION_RELATIONSHIP_WITH_TRANSFORMATION(#68)
SHAPE_REPRESENTATION_RELATIONSHIP()
);
#132=(
REPRESENTATION_RELATIONSHIP($,$,#10831,#10821)
REPRESENTATION_RELATIONSHIP_WITH_TRANSFORMATION(#69)
SHAPE_REPRESENTATION_RELATIONSHIP()
);
#133=(
REPRESENTATION_RELATIONSHIP($,$,#10795,#10794)
REPRESENTATION_RELATIONSHIP_WITH_TRANSFORMATION(#70)
SHAPE_REPRESENTATION_RELATIONSHIP()
);
#134=(
REPRESENTATION_RELATIONSHIP($,$,#10809,#10794)
REPRESENTATION_RELATIONSHIP_WITH_TRANSFORMATION(#71)
SHAPE_REPRESENTATION_RELATIONSHIP()
);
#135=(
REPRESENTATION_RELATIONSHIP($,$,#10818,#10794)
REPRESENTATION_RELATIONSHIP_WITH_TRANSFORMATION(#72)
SHAPE_REPRESENTATION_RELATIONSHIP()
);
#136=(
REPRESENTATION_RELATIONSHIP($,$,#10821,#10794)
REPRESENTATION_RELATIONSHIP_WITH_TRANSFORMATION(#73)
SHAPE_REPRESENTATION_RELATIONSHIP()
);
#137=CONTEXT_DEPENDENT_SHAPE_REPRESENTATION(#74,#10705);
#138=CONTEXT_DEPENDENT_SHAPE_REPRESENTATION(#75,#10706);
#139=CONTEXT_DEPENDENT_SHAPE_REPRESENTATION(#76,#10707);
#140=CONTEXT_DEPENDENT_SHAPE_REPRESENTATION(#77,#10708);
#141=CONTEXT_DEPENDENT_SHAPE_REPRESENTATION(#78,#10709);
#142=CONTEXT_DEPENDENT_SHAPE_REPRESENTATION(#79,#10725);
#143=CONTEXT_DEPENDENT_SHAPE_REPRESENTATION(#80,#10726);
#144=CONTEXT_DEPENDENT_SHAPE_REPRESENTATION(#81,#10727);
#145=CONTEXT_DEPENDENT_SHAPE_REPRESENTATION(#82,#10735);
#146=CONTEXT_DEPENDENT_SHAPE_REPRESENTATION(#83,#10736);
#147=CONTEXT_DEPENDENT_SHAPE_REPRESENTATION(#84,#10741);
#148=CONTEXT_DEPENDENT_SHAPE_REPRESENTATION(#85,#10742);
#149=CONTEXT_DEPENDENT_SHAPE_REPRESENTATION(#86,#10743);
#150=CONTEXT_DEPENDENT_SHAPE_REPRESENTATION(#87,#10744);
#151=CONTEXT_DEPENDENT_SHAPE_REPRESENTATION(#88,#10745);
#152=CONTEXT_DEPENDENT_SHAPE_REPRESENTATION(#89,#10746);
#153=CONTEXT_DEPENDENT_SHAPE_REPRESENTATION(#90,#10747);
#154=CONTEXT_DEPENDENT_SHAPE_REPRESENTATION(#91,#10748);
#155=CONTEXT_DEPENDENT_SHAPE_REPRESENTATION(#92,#10749);
#156=CONTEXT_DEPENDENT_SHAPE_REPRESENTATION(#93,#10750);
#157=CONTEXT_DEPENDENT_SHAPE_REPRESENTATION(#94,#10751);
#158=CONTEXT_DEPENDENT_SHAPE_REPRESENTATION(#95,#10752);
#159=CONTEXT_DEPENDENT_SHAPE_REPRESENTATION(#96,#10753);
#160=CONTEXT_DEPENDENT_SHAPE_REPRESENTATION(#97,#10754);
#161=CONTEXT_DEPENDENT_SHAPE_REPRESENTATION(#98,#10755);
#162=CONTEXT_DEPENDENT_SHAPE_REPRESENTATION(#99,#10756);
#163=CONTEXT_DEPENDENT_SHAPE_REPRESENTATION(#100,#10757);
#164=CONTEXT_DEPENDENT_SHAPE_REPRESENTATION(#101,#10758);
#165=CONTEXT_DEPENDENT_SHAPE_REPRESENTATION(#102,#10759);
#166=CONTEXT_DEPENDENT_SHAPE_REPRESENTATION(#103,#10760);
#167=CONTEXT_DEPENDENT_SHAPE_REPRESENTATION(#104,#10761);
#168=CONTEXT_DEPENDENT_SHAPE_REPRESENTATION(#105,#10762);
#169=CONTEXT_DEPENDENT_SHAPE_REPRESENTATION(#106,#10763);
#170=CONTEXT_DEPENDENT_SHAPE_REPRESENTATION(#107,#10764);
#171=CONTEXT_DEPENDENT_SHAPE_REPRESENTATION(#108,#10765);
#172=CONTEXT_DEPENDENT_SHAPE_REPRESENTATION(#109,#10766);
#173=CONTEXT_DEPENDENT_SHAPE_REPRESENTATION(#110,#10767);
#174=CONTEXT_DEPENDENT_SHAPE_REPRESENTATION(#111,#10768);
#175=CONTEXT_DEPENDENT_SHAPE_REPRESENTATION(#112,#10769);
#176=CONTEXT_DEPENDENT_SHAPE_REPRESENTATION(#113,#10770);
#177=CONTEXT_DEPENDENT_SHAPE_REPRESENTATION(#114,#10771);
#178=CONTEXT_DEPENDENT_SHAPE_REPRESENTATION(#115,#10772);
#179=CONTEXT_DEPENDENT_SHAPE_REPRESENTATION(#116,#10773);
#180=CONTEXT_DEPENDENT_SHAPE_REPRESENTATION(#117,#10774);
#181=CONTEXT_DEPENDENT_SHAPE_REPRESENTATION(#118,#10775);
#182=CONTEXT_DEPENDENT_SHAPE_REPRESENTATION(#119,#10776);
#183=CONTEXT_DEPENDENT_SHAPE_REPRESENTATION(#120,#10777);
#184=CONTEXT_DEPENDENT_SHAPE_REPRESENTATION(#121,#10778);
#185=CONTEXT_DEPENDENT_SHAPE_REPRESENTATION(#122,#10779);
#186=CONTEXT_DEPENDENT_SHAPE_REPRESENTATION(#123,#10780);
#187=CONTEXT_DEPENDENT_SHAPE_REPRESENTATION(#124,#10781);
#188=CONTEXT_DEPENDENT_SHAPE_REPRESENTATION(#125,#10782);
#189=CONTEXT_DEPENDENT_SHAPE_REPRESENTATION(#126,#10783);
#190=CONTEXT_DEPENDENT_SHAPE_REPRESENTATION(#127,#10784);
#191=CONTEXT_DEPENDENT_SHAPE_REPRESENTATION(#128,#10785);
#192=CONTEXT_DEPENDENT_SHAPE_REPRESENTATION(#129,#10786);
#193=CONTEXT_DEPENDENT_SHAPE_REPRESENTATION(#130,#10787);
#194=CONTEXT_DEPENDENT_SHAPE_REPRESENTATION(#131,#10788);
#195=CONTEXT_DEPENDENT_SHAPE_REPRESENTATION(#132,#10789);
#196=CONTEXT_DEPENDENT_SHAPE_REPRESENTATION(#133,#10790);
#197=CONTEXT_DEPENDENT_SHAPE_REPRESENTATION(#134,#10791);
#198=CONTEXT_DEPENDENT_SHAPE_REPRESENTATION(#135,#10792);
#199=CONTEXT_DEPENDENT_SHAPE_REPRESENTATION(#136,#10793);
#200=NEXT_ASSEMBLY_USAGE_OCCURRENCE('Inner ring:1','Inner ring:1',
'Inner ring:1',#10839,#10840,'Inner ring:1');
#201=NEXT_ASSEMBLY_USAGE_OCCURRENCE('Outer ring:1','Outer ring:1',
'Outer ring:1',#10839,#10841,'Outer ring:1');
#202=NEXT_ASSEMBLY_USAGE_OCCURRENCE('Balls:1','Balls:1','Balls:1',#10839,
#10842,'Balls:1');
#203=NEXT_ASSEMBLY_USAGE_OCCURRENCE('Cage:1','Cage:1','Cage:1',#10839,#10843,
'Cage:1');
#204=NEXT_ASSEMBLY_USAGE_OCCURRENCE('Seals 2RS:1','Seals 2RS:1',
'Seals 2RS:1',#10839,#10844,'Seals 2RS:1');
#205=NEXT_ASSEMBLY_USAGE_OCCURRENCE('Offset connecting link:1',
'Offset connecting link:1','Offset connecting link:1',#10857,#10858,
'Offset connecting link:1');
#206=NEXT_ASSEMBLY_USAGE_OCCURRENCE('Plain link bushing:2',
'Plain link bushing:2','Plain link bushing:2',#10857,#10859,
'Plain link bushing:2');
#207=NEXT_ASSEMBLY_USAGE_OCCURRENCE('Plain link bushing:3',
'Plain link bushing:3','Plain link bushing:3',#10857,#10859,
'Plain link bushing:3');
#208=NEXT_ASSEMBLY_USAGE_OCCURRENCE('Steel sleeve:1','Steel sleeve:1',
'Steel sleeve:1',#10864,#10865,'Steel sleeve:1');
#209=NEXT_ASSEMBLY_USAGE_OCCURRENCE('Ball retainer (plastic):1',
'Ball retainer (plastic):1','Ball retainer (plastic):1',#10864,#10866,
'Ball retainer (plastic):1');
#210=NEXT_ASSEMBLY_USAGE_OCCURRENCE('Demonstrator base:1',
'Demonstrator base:1','Demonstrator base:1',#10834,#10835,
'Demonstrator base:1');
#211=NEXT_ASSEMBLY_USAGE_OCCURRENCE('M5x14 Cap Screw:2',
'M5x14 Cap Screw:2','M5x14 Cap Screw:2',#10834,#10836,
'M5x14 Cap Screw:2');
#212=NEXT_ASSEMBLY_USAGE_OCCURRENCE('M5x14 Cap Screw:3',
'M5x14 Cap Screw:3','M5x14 Cap Screw:3',#10834,#10836,
'M5x14 Cap Screw:3');
#213=NEXT_ASSEMBLY_USAGE_OCCURRENCE('M5x14 Cap Screw:4',
'M5x14 Cap Screw:4','M5x14 Cap Screw:4',#10834,#10836,
'M5x14 Cap Screw:4');
#214=NEXT_ASSEMBLY_USAGE_OCCURRENCE('M5x14 Cap Screw:5',
'M5x14 Cap Screw:5','M5x14 Cap Screw:5',#10834,#10836,
'M5x14 Cap Screw:5');
#215=NEXT_ASSEMBLY_USAGE_OCCURRENCE('Pivot pedestal:2',
'Pivot pedestal:2','Pivot pedestal:2',#10834,#10837,'Pivot pedestal:2');
#216=NEXT_ASSEMBLY_USAGE_OCCURRENCE('Pivot cap:2','Pivot cap:2',
'Pivot cap:2',#10834,#10838,'Pivot cap:2');
#217=NEXT_ASSEMBLY_USAGE_OCCURRENCE(
'Sealed Ball Bearing - 10 x 30 x 9 mm:2',
'Sealed Ball Bearing - 10 x 30 x 9 mm:2',
'Sealed Ball Bearing - 10 x 30 x 9 mm:2',#10834,#10839,
'Sealed Ball Bearing - 10 x 30 x 9 mm:2');
#218=NEXT_ASSEMBLY_USAGE_OCCURRENCE('M4x10 Cap Screw:2',
'M4x10 Cap Screw:2','M4x10 Cap Screw:2',#10834,#10870,
'M4x10 Cap Screw:2');
#219=NEXT_ASSEMBLY_USAGE_OCCURRENCE('M4x10 Cap Screw:3',
'M4x10 Cap Screw:3','M4x10 Cap Screw:3',#10834,#10870,
'M4x10 Cap Screw:3');
#220=NEXT_ASSEMBLY_USAGE_OCCURRENCE('M4x10 Cap Screw:4',
'M4x10 Cap Screw:4','M4x10 Cap Screw:4',#10834,#10870,
'M4x10 Cap Screw:4');
#221=NEXT_ASSEMBLY_USAGE_OCCURRENCE('M4x10 Cap Screw:5',
'M4x10 Cap Screw:5','M4x10 Cap Screw:5',#10834,#10870,
'M4x10 Cap Screw:5');
#222=NEXT_ASSEMBLY_USAGE_OCCURRENCE('Eighty millimetre guide shaft:2',
'Eighty millimetre guide shaft:2','Eighty millimetre guide shaft:2',#10834,
#10845,'Eighty millimetre guide shaft:2');
#223=NEXT_ASSEMBLY_USAGE_OCCURRENCE('Horizontal shaft support:2',
'Horizontal shaft support:2','Horizontal shaft support:2',#10834,#10846,
'Horizontal shaft support:2');
#224=NEXT_ASSEMBLY_USAGE_OCCURRENCE('Cap Screw - M4x16:3',
'Cap Screw - M4x16:3','Cap Screw - M4x16:3',#10834,#10853,
'Cap Screw - M4x16:3');
#225=NEXT_ASSEMBLY_USAGE_OCCURRENCE('Cap Screw - M4x16:4',
'Cap Screw - M4x16:4','Cap Screw - M4x16:4',#10834,#10853,
'Cap Screw - M4x16:4');
#226=NEXT_ASSEMBLY_USAGE_OCCURRENCE('Socket Set Screw - M4x6:2',
'Socket Set Screw - M4x6:2','Socket Set Screw - M4x6:2',#10834,#10847,
'Socket Set Screw - M4x6:2');
#227=NEXT_ASSEMBLY_USAGE_OCCURRENCE('Horizontal shaft support:3',
'Horizontal shaft support:3','Horizontal shaft support:3',#10834,#10846,
'Horizontal shaft support:3');
#228=NEXT_ASSEMBLY_USAGE_OCCURRENCE('Cap Screw - M4x16:5',
'Cap Screw - M4x16:5','Cap Screw - M4x16:5',#10834,#10853,
'Cap Screw - M4x16:5');
#229=NEXT_ASSEMBLY_USAGE_OCCURRENCE('Cap Screw - M4x16:6',
'Cap Screw - M4x16:6','Cap Screw - M4x16:6',#10834,#10853,
'Cap Screw - M4x16:6');
#230=NEXT_ASSEMBLY_USAGE_OCCURRENCE('Socket Set Screw - M4x6:3',
'Socket Set Screw - M4x6:3','Socket Set Screw - M4x6:3',#10834,#10847,
'Socket Set Screw - M4x6:3');
#231=NEXT_ASSEMBLY_USAGE_OCCURRENCE('Bell crank and spindle:2',
'Bell crank and spindle:2','Bell crank and spindle:2',#10848,#10849,
'Bell crank and spindle:2');
#232=NEXT_ASSEMBLY_USAGE_OCCURRENCE('Input grip:2','Input grip:2',
'Input grip:2',#10848,#10850,'Input grip:2');
#233=NEXT_ASSEMBLY_USAGE_OCCURRENCE('Lower race sleeve:2',
'Lower race sleeve:2','Lower race sleeve:2',#10848,#10851,
'Lower race sleeve:2');
#234=NEXT_ASSEMBLY_USAGE_OCCURRENCE('Spindle collar:2',
'Spindle collar:2','Spindle collar:2',#10848,#10852,'Spindle collar:2');
#235=NEXT_ASSEMBLY_USAGE_OCCURRENCE('Cap Screw - M4x16:2',
'Cap Screw - M4x16:2','Cap Screw - M4x16:2',#10848,#10853,
'Cap Screw - M4x16:2');
#236=NEXT_ASSEMBLY_USAGE_OCCURRENCE('M4x4 collar screw:2',
'M4x4 collar screw:2','M4x4 collar screw:2',#10848,#10854,
'M4x4 collar screw:2');
#237=NEXT_ASSEMBLY_USAGE_OCCURRENCE('Horizontal link pin:2',
'Horizontal link pin:2','Horizontal link pin:2',#10848,#10855,
'Horizontal link pin:2');
#238=NEXT_ASSEMBLY_USAGE_OCCURRENCE('Horizontal lower pin sleeve:2',
'Horizontal lower pin sleeve:2','Horizontal lower pin sleeve:2',#10848,
#10856,'Horizontal lower pin sleeve:2');
#239=NEXT_ASSEMBLY_USAGE_OCCURRENCE('Upper pin sleeve:2',
'Upper pin sleeve:2','Upper pin sleeve:2',#10848,#10868,
'Upper pin sleeve:2');
#240=NEXT_ASSEMBLY_USAGE_OCCURRENCE('Pin keeper:2','Pin keeper:2',
'Pin keeper:2',#10848,#10869,'Pin keeper:2');
#241=NEXT_ASSEMBLY_USAGE_OCCURRENCE('M4x10 Cap Screw:14',
'M4x10 Cap Screw:14','M4x10 Cap Screw:14',#10848,#10870,
'M4x10 Cap Screw:14');
#242=NEXT_ASSEMBLY_USAGE_OCCURRENCE('Carriage link pin:1',
'Carriage link pin:1','Carriage link pin:1',#10860,#10861,
'Carriage link pin:1');
#243=NEXT_ASSEMBLY_USAGE_OCCURRENCE('Carriage pin sleeve:1',
'Carriage pin sleeve:1','Carriage pin sleeve:1',#10860,#10862,
'Carriage pin sleeve:1');
#244=NEXT_ASSEMBLY_USAGE_OCCURRENCE('Horizontal output housing:2',
'Horizontal output housing:2','Horizontal output housing:2',#10860,#10863,
'Horizontal output housing:2');
#245=NEXT_ASSEMBLY_USAGE_OCCURRENCE(
'Linear Ball Bushing - 12 x 21 x 30 mm:2',
'Linear Ball Bushing - 12 x 21 x 30 mm:2',
'Linear Ball Bushing - 12 x 21 x 30 mm:2',#10860,#10864,
'Linear Ball Bushing - 12 x 21 x 30 mm:2');
#246=NEXT_ASSEMBLY_USAGE_OCCURRENCE('Horizontal guide cap:2',
'Horizontal guide cap:2','Horizontal guide cap:2',#10860,#10867,
'Horizontal guide cap:2');
#247=NEXT_ASSEMBLY_USAGE_OCCURRENCE('Horizontal guide cap:3',
'Horizontal guide cap:3','Horizontal guide cap:3',#10860,#10867,
'Horizontal guide cap:3');
#248=NEXT_ASSEMBLY_USAGE_OCCURRENCE('M4x10 Cap Screw:6',
'M4x10 Cap Screw:6','M4x10 Cap Screw:6',#10860,#10870,
'M4x10 Cap Screw:6');
#249=NEXT_ASSEMBLY_USAGE_OCCURRENCE('M4x10 Cap Screw:7',
'M4x10 Cap Screw:7','M4x10 Cap Screw:7',#10860,#10870,
'M4x10 Cap Screw:7');
#250=NEXT_ASSEMBLY_USAGE_OCCURRENCE('M4x10 Cap Screw:8',
'M4x10 Cap Screw:8','M4x10 Cap Screw:8',#10860,#10870,
'M4x10 Cap Screw:8');
#251=NEXT_ASSEMBLY_USAGE_OCCURRENCE('M4x10 Cap Screw:9',
'M4x10 Cap Screw:9','M4x10 Cap Screw:9',#10860,#10870,
'M4x10 Cap Screw:9');
#252=NEXT_ASSEMBLY_USAGE_OCCURRENCE('M4x10 Cap Screw:10',
'M4x10 Cap Screw:10','M4x10 Cap Screw:10',#10860,#10870,
'M4x10 Cap Screw:10');
#253=NEXT_ASSEMBLY_USAGE_OCCURRENCE('M4x10 Cap Screw:11',
'M4x10 Cap Screw:11','M4x10 Cap Screw:11',#10860,#10870,
'M4x10 Cap Screw:11');
#254=NEXT_ASSEMBLY_USAGE_OCCURRENCE('M4x10 Cap Screw:12',
'M4x10 Cap Screw:12','M4x10 Cap Screw:12',#10860,#10870,
'M4x10 Cap Screw:12');
#255=NEXT_ASSEMBLY_USAGE_OCCURRENCE('M4x10 Cap Screw:13',
'M4x10 Cap Screw:13','M4x10 Cap Screw:13',#10860,#10870,
'M4x10 Cap Screw:13');
#256=NEXT_ASSEMBLY_USAGE_OCCURRENCE('Upper pin sleeve:3',
'Upper pin sleeve:3','Upper pin sleeve:3',#10860,#10868,
'Upper pin sleeve:3');
#257=NEXT_ASSEMBLY_USAGE_OCCURRENCE('Pin keeper:3','Pin keeper:3',
'Pin keeper:3',#10860,#10869,'Pin keeper:3');
#258=NEXT_ASSEMBLY_USAGE_OCCURRENCE('M4x10 Cap Screw:15',
'M4x10 Cap Screw:15','M4x10 Cap Screw:15',#10860,#10870,
'M4x10 Cap Screw:15');
#259=NEXT_ASSEMBLY_USAGE_OCCURRENCE('Base and guide:1',
'Base and guide:1','Base and guide:1',#10833,#10834,'Base and guide:1');
#260=NEXT_ASSEMBLY_USAGE_OCCURRENCE('Bell crank:1','Bell crank:1',
'Bell crank:1',#10833,#10848,'Bell crank:1');
#261=NEXT_ASSEMBLY_USAGE_OCCURRENCE('Connecting link:1',
'Connecting link:1','Connecting link:1',#10833,#10857,
'Connecting link:1');
#262=NEXT_ASSEMBLY_USAGE_OCCURRENCE('Output slider:1','Output slider:1',
'Output slider:1',#10833,#10860,'Output slider:1');
#263=SPHERICAL_SURFACE('',#6125,0.23815);
#264=SPHERICAL_SURFACE('',#6127,0.23815);
#265=SPHERICAL_SURFACE('',#6129,0.23815);
#266=SPHERICAL_SURFACE('',#6131,0.23815);
#267=SPHERICAL_SURFACE('',#6133,0.23815);
#268=SPHERICAL_SURFACE('',#6135,0.23815);
#269=SPHERICAL_SURFACE('',#6137,0.23815);
#270=SPHERICAL_SURFACE('',#6139,0.23815);
#271=SPHERICAL_SURFACE('',#6142,0.247676);
#272=SPHERICAL_SURFACE('',#6158,0.247676);
#273=SPHERICAL_SURFACE('',#6163,0.247676);
#274=SPHERICAL_SURFACE('',#6168,0.247676);
#275=SPHERICAL_SURFACE('',#6173,0.247676);
#276=SPHERICAL_SURFACE('',#6178,0.247676);
#277=SPHERICAL_SURFACE('',#6183,0.247676);
#278=SPHERICAL_SURFACE('',#6191,0.247676);
#279=TOROIDAL_SURFACE('',#6085,1.,0.247676);
#280=TOROIDAL_SURFACE('',#6105,1.,0.247676);
#281=B_SPLINE_CURVE_WITH_KNOTS('',3,(#8659,#8660,#8661,#8662,#8663,#8664,
#8665,#8666,#8667,#8668),.UNSPECIFIED.,.F.,.F.,(4,2,2,2,4),(0.,0.0945941824764479,
0.189188364952896,0.283770357603024,0.378352350253152),.UNSPECIFIED.);
#282=B_SPLINE_CURVE_WITH_KNOTS('',3,(#8669,#8670,#8671,#8672,#8673,#8674,
#8675,#8676,#8677,#8678,#8679,#8680,#8681,#8682,#8683,#8684,#8685,#8686,
#8687,#8688,#8689,#8690,#8691,#8692,#8693,#8694),.UNSPECIFIED.,.F.,.F.,
(4,2,2,2,2,2,2,2,2,2,2,2,4),(0.378352350253152,0.47293434290328,0.567516335553408,
0.662110518029855,0.756704700506303,0.851298882982751,0.945893065459199,
1.04047505810933,1.13505705075946,1.22963904340958,1.32422103605971,1.41881521853616,
1.51340940101261),.UNSPECIFIED.);
#283=B_SPLINE_CURVE_WITH_KNOTS('',3,(#8698,#8699,#8700,#8701,#8702,#8703,
#8704,#8705,#8706,#8707,#8708,#8709,#8710,#8711,#8712,#8713,#8714,#8715,
#8716,#8717,#8718,#8719,#8720,#8721,#8722,#8723),.UNSPECIFIED.,.F.,.F.,
(4,2,2,2,2,2,2,2,2,2,2,2,4),(0.,0.0942186410044058,0.188437282008812,0.282655768798837,
0.376874255588861,0.471092742378886,0.565311229168911,0.659529870173317,
0.753748511177723,0.847967152182129,0.942185793186535,1.03640427997656,
1.13062276676658),.UNSPECIFIED.);
#284=B_SPLINE_CURVE_WITH_KNOTS('',3,(#8724,#8725,#8726,#8727,#8728,#8729,
#8730,#8731,#8732,#8733),.UNSPECIFIED.,.F.,.F.,(4,2,2,2,4),(1.13062276676658,
1.22484125355661,1.31905974034663,1.41327838135104,1.50749702235545),
 .UNSPECIFIED.);
#285=B_SPLINE_CURVE_WITH_KNOTS('',3,(#9044,#9045,#9046,#9047,#9048,#9049,
#9050,#9051,#9052,#9053,#9054,#9055,#9056,#9057,#9058,#9059,#9060,#9061,
#9062,#9063,#9064,#9065),.UNSPECIFIED.,.F.,.F.,(4,2,2,2,2,2,2,2,2,2,4),
(0.0473477652366656,0.126350602536658,0.189525903804987,0.252701205073317,
0.313298422430275,0.373895639787233,0.434492857144191,0.495090074501149,
0.558265375769478,0.621440677037807,0.7004435143378),.UNSPECIFIED.);
#286=B_SPLINE_CURVE_WITH_KNOTS('',3,(#9069,#9070,#9071,#9072,#9073,#9074,
#9075,#9076,#9077,#9078,#9079,#9080,#9081,#9082,#9083,#9084,#9085,#9086,
#9087,#9088,#9089,#9090),.UNSPECIFIED.,.F.,.F.,(4,2,2,2,2,2,2,2,2,2,4),
(0.0464897534940957,0.0852567806515119,0.170513561303024,0.246687263103517,
0.308657850341199,0.370628437578881,0.432599024816563,0.494569612054245,
0.570743313854739,0.656000094506251,0.694767121663666),.UNSPECIFIED.);
#287=B_SPLINE_CURVE_WITH_KNOTS('',3,(#9096,#9097,#9098,#9099,#9100,#9101,
#9102,#9103,#9104,#9105,#9106,#9107,#9108,#9109,#9110,#9111,#9112,#9113,
#9114,#9115,#9116,#9117),.UNSPECIFIED.,.F.,.F.,(4,2,2,2,2,2,2,2,2,2,4),
(0.0464897534940957,0.0852567806515118,0.170513561303024,0.246687263103517,
0.308657850341199,0.370628437578881,0.432599024816563,0.494569612054245,
0.570743313854738,0.65600009450625,0.694767121663666),.UNSPECIFIED.);
#288=B_SPLINE_CURVE_WITH_KNOTS('',3,(#9121,#9122,#9123,#9124,#9125,#9126,
#9127,#9128,#9129,#9130,#9131,#9132,#9133,#9134,#9135,#9136,#9137,#9138,
#9139,#9140,#9141,#9142),.UNSPECIFIED.,.F.,.F.,(4,2,2,2,2,2,2,2,2,2,4),
(0.0464897534940957,0.0852567806515119,0.170513561303024,0.246687263103517,
0.308657850341199,0.370628437578881,0.432599024816563,0.494569612054245,
0.570743313854739,0.656000094506251,0.694767121663666),.UNSPECIFIED.);
#289=B_SPLINE_CURVE_WITH_KNOTS('',3,(#9146,#9147,#9148,#9149,#9150,#9151,
#9152,#9153,#9154,#9155,#9156,#9157),.UNSPECIFIED.,.F.,.F.,(4,2,2,2,2,4),
(0.0464897534940957,0.0852567806515119,0.170513561303024,0.246687263103517,
0.308657850341199,0.370628437578881),.UNSPECIFIED.);
#290=B_SPLINE_CURVE_WITH_KNOTS('',3,(#9162,#9163,#9164,#9165,#9166,#9167,
#9168,#9169,#9170,#9171,#9172,#9173),.UNSPECIFIED.,.F.,.F.,(4,2,2,2,2,4),
(0.370628437578881,0.432599024816563,0.494569612054245,0.570743313854738,
0.65600009450625,0.694767121663666),.UNSPECIFIED.);
#291=B_SPLINE_CURVE_WITH_KNOTS('',3,(#9177,#9178,#9179,#9180,#9181,#9182,
#9183,#9184,#9185,#9186,#9187,#9188,#9189,#9190,#9191,#9192,#9193,#9194,
#9195,#9196,#9197,#9198),.UNSPECIFIED.,.F.,.F.,(4,2,2,2,2,2,2,2,2,2,4),
(0.0464897534940957,0.0852567806515121,0.170513561303024,0.246687263103518,
0.308657850341199,0.370628437578881,0.432599024816563,0.494569612054245,
0.570743313854738,0.65600009450625,0.694767121663666),.UNSPECIFIED.);
#292=B_SPLINE_CURVE_WITH_KNOTS('',3,(#9202,#9203,#9204,#9205,#9206,#9207,
#9208,#9209,#9210,#9211,#9212,#9213,#9214,#9215,#9216,#9217,#9218,#9219,
#9220,#9221,#9222,#9223),.UNSPECIFIED.,.F.,.F.,(4,2,2,2,2,2,2,2,2,2,4),
(0.0464897534940957,0.0852567806515119,0.170513561303024,0.246687263103517,
0.308657850341199,0.370628437578881,0.432599024816563,0.494569612054245,
0.570743313854738,0.65600009450625,0.694767121663667),.UNSPECIFIED.);
#293=B_SPLINE_CURVE_WITH_KNOTS('',3,(#9227,#9228,#9229,#9230,#9231,#9232,
#9233,#9234,#9235,#9236,#9237,#9238,#9239,#9240,#9241,#9242,#9243,#9244,
#9245,#9246,#9247,#9248),.UNSPECIFIED.,.F.,.F.,(4,2,2,2,2,2,2,2,2,2,4),
(0.0464897534940957,0.0852567806515119,0.170513561303024,0.246687263103517,
0.308657850341199,0.370628437578881,0.432599024816563,0.494569612054245,
0.570743313854738,0.65600009450625,0.694767121663666),.UNSPECIFIED.);
#294=B_SPLINE_CURVE_WITH_KNOTS('',3,(#9252,#9253,#9254,#9255,#9256,#9257,
#9258,#9259,#9260,#9261,#9262,#9263,#9264,#9265,#9266,#9267,#9268,#9269,
#9270,#9271,#9272,#9273),.UNSPECIFIED.,.F.,.F.,(4,2,2,2,2,2,2,2,2,2,4),
(0.0464897534940957,0.0852567806515119,0.170513561303024,0.246687263103517,
0.308657850341199,0.370628437578881,0.432599024816563,0.494569612054245,
0.570743313854739,0.656000094506251,0.694767121663667),.UNSPECIFIED.);
#295=B_SPLINE_CURVE_WITH_KNOTS('',3,(#9281,#9282,#9283,#9284,#9285,#9286,
#9287,#9288,#9289,#9290,#9291,#9292,#9293,#9294,#9295,#9296,#9297,#9298,
#9299,#9300,#9301,#9302),.UNSPECIFIED.,.F.,.F.,(4,2,2,2,2,2,2,2,2,2,4),
(0.0473477652366656,0.126350602536658,0.189525903804987,0.252701205073316,
0.313298422430274,0.373895639787232,0.434492857144191,0.495090074501149,
0.558265375769478,0.621440677037807,0.7004435143378),.UNSPECIFIED.);
#296=B_SPLINE_CURVE_WITH_KNOTS('',3,(#9310,#9311,#9312,#9313,#9314,#9315,
#9316,#9317,#9318,#9319,#9320,#9321,#9322,#9323,#9324,#9325,#9326,#9327,
#9328,#9329,#9330,#9331),.UNSPECIFIED.,.F.,.F.,(4,2,2,2,2,2,2,2,2,2,4),
(0.0473477652366656,0.126350602536658,0.189525903804987,0.252701205073317,
0.313298422430275,0.373895639787233,0.434492857144191,0.495090074501149,
0.558265375769478,0.621440677037807,0.7004435143378),.UNSPECIFIED.);
#297=B_SPLINE_CURVE_WITH_KNOTS('',3,(#9340,#9341,#9342,#9343,#9344,#9345,
#9346,#9347,#9348,#9349,#9350,#9351),.UNSPECIFIED.,.F.,.F.,(4,2,2,2,2,4),
(0.0473477652366656,0.126350602536658,0.189525903804987,0.252701205073316,
0.313298422430275,0.373895639787233),.UNSPECIFIED.);
#298=B_SPLINE_CURVE_WITH_KNOTS('',3,(#9353,#9354,#9355,#9356,#9357,#9358,
#9359,#9360,#9361,#9362,#9363,#9364),.UNSPECIFIED.,.F.,.F.,(4,2,2,2,2,4),
(0.373895639787233,0.434492857144191,0.495090074501149,0.558265375769478,
0.621440677037807,0.7004435143378),.UNSPECIFIED.);
#299=B_SPLINE_CURVE_WITH_KNOTS('',3,(#9371,#9372,#9373,#9374,#9375,#9376,
#9377,#9378,#9379,#9380,#9381,#9382,#9383,#9384,#9385,#9386,#9387,#9388,
#9389,#9390,#9391,#9392),.UNSPECIFIED.,.F.,.F.,(4,2,2,2,2,2,2,2,2,2,4),
(0.0473477652366656,0.126350602536658,0.189525903804987,0.252701205073316,
0.313298422430275,0.373895639787233,0.434492857144191,0.495090074501149,
0.558265375769478,0.621440677037807,0.7004435143378),.UNSPECIFIED.);
#300=B_SPLINE_CURVE_WITH_KNOTS('',3,(#9400,#9401,#9402,#9403,#9404,#9405,
#9406,#9407,#9408,#9409,#9410,#9411,#9412,#9413,#9414,#9415,#9416,#9417,
#9418,#9419,#9420,#9421),.UNSPECIFIED.,.F.,.F.,(4,2,2,2,2,2,2,2,2,2,4),
(0.0473477652366656,0.126350602536658,0.189525903804987,0.252701205073317,
0.313298422430275,0.373895639787233,0.434492857144191,0.495090074501149,
0.558265375769478,0.621440677037807,0.7004435143378),.UNSPECIFIED.);
#301=B_SPLINE_CURVE_WITH_KNOTS('',3,(#9429,#9430,#9431,#9432,#9433,#9434,
#9435,#9436,#9437,#9438,#9439,#9440,#9441,#9442,#9443,#9444,#9445,#9446,
#9447,#9448,#9449,#9450),.UNSPECIFIED.,.F.,.F.,(4,2,2,2,2,2,2,2,2,2,4),
(0.0473477652366656,0.126350602536658,0.189525903804987,0.252701205073316,
0.313298422430275,0.373895639787233,0.434492857144191,0.495090074501149,
0.558265375769478,0.621440677037807,0.7004435143378),.UNSPECIFIED.);
#302=B_SPLINE_CURVE_WITH_KNOTS('',3,(#9459,#9460,#9461,#9462,#9463,#9464,
#9465,#9466,#9467,#9468,#9469,#9470,#9471,#9472,#9473,#9474,#9475,#9476,
#9477,#9478,#9479,#9480),.UNSPECIFIED.,.F.,.F.,(4,2,2,2,2,2,2,2,2,2,4),
(0.0473477652366656,0.126350602536658,0.189525903804987,0.252701205073317,
0.313298422430275,0.373895639787233,0.434492857144191,0.495090074501149,
0.558265375769478,0.621440677037807,0.7004435143378),.UNSPECIFIED.);
#303=B_SPLINE_CURVE_WITH_KNOTS('',3,(#9562,#9563,#9564,#9565,#9566,#9567),
 .UNSPECIFIED.,.F.,.F.,(4,2,4),(0.635430324955934,0.687528937234029,0.750024497760675),
 .UNSPECIFIED.);
#304=B_SPLINE_CURVE_WITH_KNOTS('',3,(#9571,#9572,#9573,#9574,#9575,#9576),
 .UNSPECIFIED.,.F.,.F.,(4,2,4),(0.250008165920225,0.312503726446871,0.364602338724967),
 .UNSPECIFIED.);
#305=B_SPLINE_CURVE_WITH_KNOTS('',3,(#9577,#9578,#9579,#9580,#9581,#9582),
 .UNSPECIFIED.,.F.,.F.,(4,2,4),(0.135413993115484,0.187512605393579,0.250008165920225),
 .UNSPECIFIED.);
#306=B_SPLINE_CURVE_WITH_KNOTS('',3,(#9583,#9584,#9585,#9586,#9587,#9588),
 .UNSPECIFIED.,.F.,.F.,(4,2,4),(0.750024497760675,0.81252005828732,0.864618670565416),
 .UNSPECIFIED.);
#307=B_SPLINE_CURVE_WITH_KNOTS('',3,(#9836,#9837,#9838,#9839,#9840,#9841,
#9842,#9843,#9844,#9845,#9846,#9847,#9848,#9849),.UNSPECIFIED.,.F.,.F.,
(4,2,2,2,2,2,4),(0.618551524396293,0.626563103102765,0.689203386094988,
0.751843669087211,0.814483952079434,0.877124235071657,0.88513581377813),
 .UNSPECIFIED.);
#308=B_SPLINE_CURVE_WITH_KNOTS('',3,(#9853,#9854,#9855,#9856,#9857,#9858,
#9859,#9860),.UNSPECIFIED.,.F.,.F.,(4,2,2,4),(0.250614556362404,0.313254839354627,
0.37589512234685,0.383906701053323),.UNSPECIFIED.);
#309=B_SPLINE_CURVE_WITH_KNOTS('',3,(#9864,#9865,#9866,#9867,#9868,#9869,
#9870,#9871,#9872,#9873,#9874,#9875,#9876,#9877,#9878,#9879,#9880,#9881,
#9882,#9883,#9884,#9885,#9886,#9887,#9888,#9889),.UNSPECIFIED.,.F.,.F.,
(4,2,2,2,2,2,2,2,2,2,2,2,4),(0.,0.0623062782223143,0.124612556444629,0.186916384615149,
0.249220212785669,0.31152404095619,0.37382786912671,0.436134147349024,0.498440425571339,
0.560746703793653,0.623052982015967,0.685356810186488,0.747660638357008),
 .UNSPECIFIED.);
#310=B_SPLINE_CURVE_WITH_KNOTS('',3,(#9890,#9891,#9892,#9893,#9894,#9895,
#9896,#9897,#9898,#9899),.UNSPECIFIED.,.F.,.F.,(4,2,2,2,4),(0.747660638357008,
0.809964466527528,0.872268294698049,0.934574572920363,0.996880851142677),
 .UNSPECIFIED.);
#311=B_SPLINE_CURVE_WITH_KNOTS('',3,(#9900,#9901,#9902,#9903,#9904,#9905,
#9906,#9907),.UNSPECIFIED.,.F.,.F.,(4,2,2,4),(0.117322411671485,0.125333990377958,
0.187974273370181,0.250614556362404),.UNSPECIFIED.);
#312=CONICAL_SURFACE('',#5961,0.4,0.785398163397448);
#313=CONICAL_SURFACE('',#5965,0.41,0.785398163397448);
#314=CONICAL_SURFACE('',#5969,0.26,0.463647609000806);
#315=CONICAL_SURFACE('',#6096,0.53,0.785398163397448);
#316=CONICAL_SURFACE('',#6103,0.53,0.785398163397448);
#317=CONICAL_SURFACE('',#6116,1.47,0.785398163397449);
#318=CONICAL_SURFACE('',#6120,1.47,0.785398163397449);
#319=CONICAL_SURFACE('',#6220,0.55,0.785398163397448);
#320=CONICAL_SURFACE('',#6265,0.185,0.785398163397449);
#321=CONICAL_SURFACE('',#6269,0.1625,0.785398163397449);
#322=CONICAL_SURFACE('',#6353,0.325,0.785398163397448);
#323=CONICAL_SURFACE('',#6357,0.335,0.785398163397448);
#324=CONICAL_SURFACE('',#6361,0.21,0.463647609000806);
#325=CONICAL_SURFACE('',#6365,0.18,0.785398163397448);
#326=CONICAL_SURFACE('',#6388,0.185,0.785398163397449);
#327=CONICAL_SURFACE('',#6607,0.325,0.785398163397448);
#328=CONICAL_SURFACE('',#6611,0.335,0.785398163397448);
#329=CONICAL_SURFACE('',#6615,0.21,0.463647609000806);
#330=ORIENTED_CLOSED_SHELL('',*,#5532,.F.);
#331=ORIENTED_CLOSED_SHELL('',*,#5557,.F.);
#332=ORIENTED_CLOSED_SHELL('',*,#5571,.F.);
#333=BREP_WITH_VOIDS('Body1',#5533,(#330));
#334=BREP_WITH_VOIDS('Body1',#5556,(#331));
#335=BREP_WITH_VOIDS('Body1',#5572,(#332));
#336=SHAPE_REPRESENTATION_RELATIONSHIP('SRR','None',#10796,#367);
#337=SHAPE_REPRESENTATION_RELATIONSHIP('SRR','None',#10797,#368);
#338=SHAPE_REPRESENTATION_RELATIONSHIP('SRR','None',#10798,#369);
#339=SHAPE_REPRESENTATION_RELATIONSHIP('SRR','None',#10799,#370);
#340=SHAPE_REPRESENTATION_RELATIONSHIP('SRR','None',#10801,#371);
#341=SHAPE_REPRESENTATION_RELATIONSHIP('SRR','None',#10802,#372);
#342=SHAPE_REPRESENTATION_RELATIONSHIP('SRR','None',#10803,#373);
#343=SHAPE_REPRESENTATION_RELATIONSHIP('SRR','None',#10804,#374);
#344=SHAPE_REPRESENTATION_RELATIONSHIP('SRR','None',#10805,#375);
#345=SHAPE_REPRESENTATION_RELATIONSHIP('SRR','None',#10806,#376);
#346=SHAPE_REPRESENTATION_RELATIONSHIP('SRR','None',#10807,#377);
#347=SHAPE_REPRESENTATION_RELATIONSHIP('SRR','None',#10808,#378);
#348=SHAPE_REPRESENTATION_RELATIONSHIP('SRR','None',#10810,#379);
#349=SHAPE_REPRESENTATION_RELATIONSHIP('SRR','None',#10811,#380);
#350=SHAPE_REPRESENTATION_RELATIONSHIP('SRR','None',#10812,#381);
#351=SHAPE_REPRESENTATION_RELATIONSHIP('SRR','None',#10813,#382);
#352=SHAPE_REPRESENTATION_RELATIONSHIP('SRR','None',#10814,#383);
#353=SHAPE_REPRESENTATION_RELATIONSHIP('SRR','None',#10815,#384);
#354=SHAPE_REPRESENTATION_RELATIONSHIP('SRR','None',#10816,#385);
#355=SHAPE_REPRESENTATION_RELATIONSHIP('SRR','None',#10817,#386);
#356=SHAPE_REPRESENTATION_RELATIONSHIP('SRR','None',#10819,#387);
#357=SHAPE_REPRESENTATION_RELATIONSHIP('SRR','None',#10820,#388);
#358=SHAPE_REPRESENTATION_RELATIONSHIP('SRR','None',#10822,#389);
#359=SHAPE_REPRESENTATION_RELATIONSHIP('SRR','None',#10823,#390);
#360=SHAPE_REPRESENTATION_RELATIONSHIP('SRR','None',#10824,#391);
#361=SHAPE_REPRESENTATION_RELATIONSHIP('SRR','None',#10826,#392);
#362=SHAPE_REPRESENTATION_RELATIONSHIP('SRR','None',#10827,#393);
#363=SHAPE_REPRESENTATION_RELATIONSHIP('SRR','None',#10828,#394);
#364=SHAPE_REPRESENTATION_RELATIONSHIP('SRR','None',#10829,#395);
#365=SHAPE_REPRESENTATION_RELATIONSHIP('SRR','None',#10830,#396);
#366=SHAPE_REPRESENTATION_RELATIONSHIP('SRR','None',#10831,#397);
#367=ADVANCED_BREP_SHAPE_REPRESENTATION('',(#437),#10614);
#368=ADVANCED_BREP_SHAPE_REPRESENTATION('',(#333),#10615);
#369=ADVANCED_BREP_SHAPE_REPRESENTATION('',(#438),#10616);
#370=ADVANCED_BREP_SHAPE_REPRESENTATION('',(#439),#10617);
#371=ADVANCED_BREP_SHAPE_REPRESENTATION('',(#440),#10619);
#372=ADVANCED_BREP_SHAPE_REPRESENTATION('',(#441),#10620);
#373=ADVANCED_BREP_SHAPE_REPRESENTATION('',(#442,#443,#444,#445,#446,#447,
#448,#449),#10621);
#374=ADVANCED_BREP_SHAPE_REPRESENTATION('',(#450),#10622);
#375=ADVANCED_BREP_SHAPE_REPRESENTATION('',(#451,#452),#10623);
#376=ADVANCED_BREP_SHAPE_REPRESENTATION('',(#453),#10624);
#377=ADVANCED_BREP_SHAPE_REPRESENTATION('',(#454),#10625);
#378=ADVANCED_BREP_SHAPE_REPRESENTATION('',(#455),#10626);
#379=ADVANCED_BREP_SHAPE_REPRESENTATION('',(#456),#10628);
#380=ADVANCED_BREP_SHAPE_REPRESENTATION('',(#457),#10629);
#381=ADVANCED_BREP_SHAPE_REPRESENTATION('',(#458),#10630);
#382=ADVANCED_BREP_SHAPE_REPRESENTATION('',(#459),#10631);
#383=ADVANCED_BREP_SHAPE_REPRESENTATION('',(#334),#10632);
#384=ADVANCED_BREP_SHAPE_REPRESENTATION('',(#460),#10633);
#385=ADVANCED_BREP_SHAPE_REPRESENTATION('',(#461),#10634);
#386=ADVANCED_BREP_SHAPE_REPRESENTATION('',(#462),#10635);
#387=ADVANCED_BREP_SHAPE_REPRESENTATION('',(#463),#10637);
#388=ADVANCED_BREP_SHAPE_REPRESENTATION('',(#464),#10638);
#389=ADVANCED_BREP_SHAPE_REPRESENTATION('',(#465),#10640);
#390=ADVANCED_BREP_SHAPE_REPRESENTATION('',(#466),#10641);
#391=ADVANCED_BREP_SHAPE_REPRESENTATION('',(#467),#10642);
#392=ADVANCED_BREP_SHAPE_REPRESENTATION('',(#468),#10644);
#393=ADVANCED_BREP_SHAPE_REPRESENTATION('',(#469),#10645);
#394=ADVANCED_BREP_SHAPE_REPRESENTATION('',(#470),#10646);
#395=ADVANCED_BREP_SHAPE_REPRESENTATION('',(#471),#10647);
#396=ADVANCED_BREP_SHAPE_REPRESENTATION('',(#472),#10648);
#397=ADVANCED_BREP_SHAPE_REPRESENTATION('',(#335),#10649);
#398=STYLED_ITEM('',(#11043),#437);
#399=STYLED_ITEM('',(#11071),#333);
#400=STYLED_ITEM('',(#11078),#438);
#401=STYLED_ITEM('',(#11050),#439);
#402=STYLED_ITEM('',(#11064),#440);
#403=STYLED_ITEM('',(#11064),#441);
#404=STYLED_ITEM('',(#11064),#442);
#405=STYLED_ITEM('',(#11064),#443);
#406=STYLED_ITEM('',(#11064),#444);
#407=STYLED_ITEM('',(#11064),#445);
#408=STYLED_ITEM('',(#11064),#446);
#409=STYLED_ITEM('',(#11064),#447);
#410=STYLED_ITEM('',(#11064),#448);
#411=STYLED_ITEM('',(#11064),#449);
#412=STYLED_ITEM('',(#11064),#450);
#413=STYLED_ITEM('',(#11064),#451);
#414=STYLED_ITEM('',(#11064),#452);
#415=STYLED_ITEM('',(#11064),#453);
#416=STYLED_ITEM('',(#11064),#454);
#417=STYLED_ITEM('',(#11071),#455);
#418=STYLED_ITEM('',(#11057),#456);
#419=STYLED_ITEM('',(#11071),#457);
#420=STYLED_ITEM('',(#11050),#458);
#421=STYLED_ITEM('',(#11057),#459);
#422=STYLED_ITEM('',(#11071),#334);
#423=STYLED_ITEM('',(#11071),#460);
#424=STYLED_ITEM('',(#11064),#461);
#425=STYLED_ITEM('',(#11064),#462);
#426=STYLED_ITEM('',(#11078),#463);
#427=STYLED_ITEM('',(#11057),#464);
#428=STYLED_ITEM('',(#11064),#465);
#429=STYLED_ITEM('',(#11064),#466);
#430=STYLED_ITEM('',(#11043),#467);
#431=STYLED_ITEM('',(#11078),#468);
#432=STYLED_ITEM('',(#11057),#469);
#433=STYLED_ITEM('',(#11057),#470);
#434=STYLED_ITEM('',(#11064),#471);
#435=STYLED_ITEM('',(#11064),#472);
#436=STYLED_ITEM('',(#11071),#335);
#437=MANIFOLD_SOLID_BREP('Body1',#5531);
#438=MANIFOLD_SOLID_BREP('Body1',#5534);
#439=MANIFOLD_SOLID_BREP('Body1',#5535);
#440=MANIFOLD_SOLID_BREP('Body1',#5536);
#441=MANIFOLD_SOLID_BREP('Body1',#5537);
#442=MANIFOLD_SOLID_BREP('Body1',#5538);
#443=MANIFOLD_SOLID_BREP('Body2',#5539);
#444=MANIFOLD_SOLID_BREP('Body3',#5540);
#445=MANIFOLD_SOLID_BREP('Body4',#5541);
#446=MANIFOLD_SOLID_BREP('Body5',#5542);
#447=MANIFOLD_SOLID_BREP('Body6',#5543);
#448=MANIFOLD_SOLID_BREP('Body7',#5544);
#449=MANIFOLD_SOLID_BREP('Body8',#5545);
#450=MANIFOLD_SOLID_BREP('Continuous crown cage',#5546);
#451=MANIFOLD_SOLID_BREP('Body1',#5547);
#452=MANIFOLD_SOLID_BREP('Body2',#5548);
#453=MANIFOLD_SOLID_BREP('Body1',#5549);
#454=MANIFOLD_SOLID_BREP('Body1',#5550);
#455=MANIFOLD_SOLID_BREP('Body1',#5551);
#456=MANIFOLD_SOLID_BREP('Body1',#5552);
#457=MANIFOLD_SOLID_BREP('Body1',#5553);
#458=MANIFOLD_SOLID_BREP('Body1',#5554);
#459=MANIFOLD_SOLID_BREP('Body1',#5555);
#460=MANIFOLD_SOLID_BREP('Body1',#5558);
#461=MANIFOLD_SOLID_BREP('Body1',#5559);
#462=MANIFOLD_SOLID_BREP('Body1',#5560);
#463=MANIFOLD_SOLID_BREP('Body1',#5561);
#464=MANIFOLD_SOLID_BREP('Body1',#5562);
#465=MANIFOLD_SOLID_BREP('Body1',#5563);
#466=MANIFOLD_SOLID_BREP('Body1',#5564);
#467=MANIFOLD_SOLID_BREP('Body1',#5565);
#468=MANIFOLD_SOLID_BREP('Body1',#5566);
#469=MANIFOLD_SOLID_BREP('Body1',#5567);
#470=MANIFOLD_SOLID_BREP('Body1',#5568);
#471=MANIFOLD_SOLID_BREP('Body1',#5569);
#472=MANIFOLD_SOLID_BREP('Body1',#5570);
#473=FACE_BOUND('',#1139,.T.);
#474=FACE_BOUND('',#1140,.T.);
#475=FACE_BOUND('',#1141,.T.);
#476=FACE_BOUND('',#1142,.T.);
#477=FACE_BOUND('',#1143,.T.);
#478=FACE_BOUND('',#1144,.T.);
#479=FACE_BOUND('',#1145,.T.);
#480=FACE_BOUND('',#1146,.T.);
#481=FACE_BOUND('',#1148,.T.);
#482=FACE_BOUND('',#1149,.T.);
#483=FACE_BOUND('',#1150,.T.);
#484=FACE_BOUND('',#1151,.T.);
#485=FACE_BOUND('',#1152,.T.);
#486=FACE_BOUND('',#1153,.T.);
#487=FACE_BOUND('',#1154,.T.);
#488=FACE_BOUND('',#1155,.T.);
#489=FACE_BOUND('',#1170,.T.);
#490=FACE_BOUND('',#1192,.T.);
#491=FACE_BOUND('',#1193,.T.);
#492=FACE_BOUND('',#1194,.T.);
#493=FACE_BOUND('',#1195,.T.);
#494=FACE_BOUND('',#1196,.T.);
#495=FACE_BOUND('',#1203,.T.);
#496=FACE_BOUND('',#1205,.T.);
#497=FACE_BOUND('',#1207,.T.);
#498=FACE_BOUND('',#1209,.T.);
#499=FACE_BOUND('',#1210,.T.);
#500=FACE_BOUND('',#1211,.T.);
#501=FACE_BOUND('',#1212,.T.);
#502=FACE_BOUND('',#1213,.T.);
#503=FACE_BOUND('',#1215,.T.);
#504=FACE_BOUND('',#1216,.T.);
#505=FACE_BOUND('',#1217,.T.);
#506=FACE_BOUND('',#1218,.T.);
#507=FACE_BOUND('',#1219,.T.);
#508=FACE_BOUND('',#1222,.T.);
#509=FACE_BOUND('',#1225,.T.);
#510=FACE_BOUND('',#1228,.T.);
#511=FACE_BOUND('',#1231,.T.);
#512=FACE_BOUND('',#1238,.T.);
#513=FACE_BOUND('',#1242,.T.);
#514=FACE_BOUND('',#1243,.T.);
#515=FACE_BOUND('',#1244,.T.);
#516=FACE_BOUND('',#1245,.T.);
#517=FACE_BOUND('',#1246,.T.);
#518=FACE_BOUND('',#1248,.T.);
#519=FACE_BOUND('',#1249,.T.);
#520=FACE_BOUND('',#1250,.T.);
#521=FACE_BOUND('',#1251,.T.);
#522=FACE_BOUND('',#1252,.T.);
#523=FACE_BOUND('',#1258,.T.);
#524=FACE_BOUND('',#1261,.T.);
#525=FACE_BOUND('',#1266,.T.);
#526=FACE_BOUND('',#1271,.T.);
#527=FACE_BOUND('',#1299,.T.);
#528=FACE_BOUND('',#1302,.T.);
#529=FACE_BOUND('',#1305,.T.);
#530=FACE_BOUND('',#1308,.T.);
#531=FACE_BOUND('',#1311,.T.);
#532=FACE_BOUND('',#1324,.T.);
#533=FACE_BOUND('',#1327,.T.);
#534=FACE_BOUND('',#1329,.T.);
#535=FACE_BOUND('',#1330,.T.);
#536=FACE_BOUND('',#1331,.T.);
#537=FACE_BOUND('',#1336,.T.);
#538=FACE_BOUND('',#1338,.T.);
#539=FACE_BOUND('',#1340,.T.);
#540=FACE_BOUND('',#1341,.T.);
#541=FACE_BOUND('',#1350,.T.);
#542=FACE_BOUND('',#1361,.T.);
#543=FACE_BOUND('',#1362,.T.);
#544=FACE_BOUND('',#1363,.T.);
#545=FACE_BOUND('',#1370,.T.);
#546=FACE_BOUND('',#1371,.T.);
#547=FACE_BOUND('',#1372,.T.);
#548=FACE_BOUND('',#1373,.T.);
#549=FACE_BOUND('',#1380,.T.);
#550=FACE_BOUND('',#1389,.T.);
#551=FACE_BOUND('',#1393,.T.);
#552=FACE_BOUND('',#1395,.T.);
#553=FACE_BOUND('',#1400,.T.);
#554=FACE_BOUND('',#1402,.T.);
#555=FACE_BOUND('',#1404,.T.);
#556=FACE_BOUND('',#1406,.T.);
#557=FACE_BOUND('',#1412,.T.);
#558=FACE_BOUND('',#1434,.T.);
#559=FACE_BOUND('',#1440,.T.);
#560=FACE_BOUND('',#1442,.T.);
#561=FACE_BOUND('',#1447,.T.);
#562=FACE_BOUND('',#1452,.T.);
#563=FACE_BOUND('',#1454,.T.);
#564=FACE_BOUND('',#1460,.T.);
#565=FACE_BOUND('',#1461,.T.);
#566=FACE_BOUND('',#1465,.T.);
#567=FACE_BOUND('',#1466,.T.);
#568=FACE_BOUND('',#1470,.T.);
#569=FACE_BOUND('',#1472,.T.);
#570=FACE_BOUND('',#1476,.T.);
#571=FACE_BOUND('',#1478,.T.);
#572=FACE_BOUND('',#1483,.T.);
#573=FACE_BOUND('',#1488,.T.);
#574=FACE_BOUND('',#1490,.T.);
#575=FACE_BOUND('',#1500,.T.);
#576=FACE_BOUND('',#1501,.T.);
#577=FACE_BOUND('',#1502,.T.);
#578=FACE_BOUND('',#1503,.T.);
#579=FACE_BOUND('',#1504,.T.);
#580=FACE_BOUND('',#1507,.T.);
#581=FACE_BOUND('',#1508,.T.);
#582=FACE_BOUND('',#1509,.T.);
#583=FACE_BOUND('',#1510,.T.);
#584=FACE_BOUND('',#1511,.T.);
#585=FACE_BOUND('',#1513,.T.);
#586=FACE_BOUND('',#1521,.T.);
#587=FACE_BOUND('',#1524,.T.);
#588=FACE_BOUND('',#1527,.T.);
#589=FACE_BOUND('',#1530,.T.);
#590=FACE_BOUND('',#1533,.T.);
#591=FACE_BOUND('',#1536,.T.);
#592=FACE_BOUND('',#1538,.T.);
#593=FACE_BOUND('',#1544,.T.);
#594=FACE_BOUND('',#1546,.T.);
#595=FACE_BOUND('',#1548,.T.);
#596=FACE_BOUND('',#1550,.T.);
#597=FACE_BOUND('',#1558,.T.);
#598=FACE_BOUND('',#1559,.T.);
#599=FACE_BOUND('',#1560,.T.);
#600=FACE_BOUND('',#1561,.T.);
#601=FACE_BOUND('',#1562,.T.);
#602=FACE_BOUND('',#1565,.T.);
#603=FACE_BOUND('',#1566,.T.);
#604=FACE_BOUND('',#1567,.T.);
#605=FACE_BOUND('',#1568,.T.);
#606=FACE_BOUND('',#1569,.T.);
#607=FACE_BOUND('',#1575,.T.);
#608=FACE_BOUND('',#1577,.T.);
#609=FACE_BOUND('',#1581,.T.);
#610=FACE_BOUND('',#1583,.T.);
#611=FACE_BOUND('',#1598,.T.);
#612=PLANE('',#5942);
#613=PLANE('',#5943);
#614=PLANE('',#5944);
#615=PLANE('',#5945);
#616=PLANE('',#5946);
#617=PLANE('',#5947);
#618=PLANE('',#5949);
#619=PLANE('',#5950);
#620=PLANE('',#5951);
#621=PLANE('',#5952);
#622=PLANE('',#5953);
#623=PLANE('',#5954);
#624=PLANE('',#5955);
#625=PLANE('',#5956);
#626=PLANE('',#5957);
#627=PLANE('',#5959);
#628=PLANE('',#5967);
#629=PLANE('',#5977);
#630=PLANE('',#5981);
#631=PLANE('',#5985);
#632=PLANE('',#5989);
#633=PLANE('',#5990);
#634=PLANE('',#5998);
#635=PLANE('',#6003);
#636=PLANE('',#6008);
#637=PLANE('',#6017);
#638=PLANE('',#6034);
#639=PLANE('',#6040);
#640=PLANE('',#6041);
#641=PLANE('',#6046);
#642=PLANE('',#6051);
#643=PLANE('',#6056);
#644=PLANE('',#6061);
#645=PLANE('',#6074);
#646=PLANE('',#6081);
#647=PLANE('',#6082);
#648=PLANE('',#6098);
#649=PLANE('',#6101);
#650=PLANE('',#6113);
#651=PLANE('',#6122);
#652=PLANE('',#6155);
#653=PLANE('',#6160);
#654=PLANE('',#6165);
#655=PLANE('',#6170);
#656=PLANE('',#6175);
#657=PLANE('',#6180);
#658=PLANE('',#6189);
#659=PLANE('',#6193);
#660=PLANE('',#6194);
#661=PLANE('',#6196);
#662=PLANE('',#6201);
#663=PLANE('',#6204);
#664=PLANE('',#6209);
#665=PLANE('',#6218);
#666=PLANE('',#6224);
#667=PLANE('',#6226);
#668=PLANE('',#6227);
#669=PLANE('',#6228);
#670=PLANE('',#6233);
#671=PLANE('',#6237);
#672=PLANE('',#6242);
#673=PLANE('',#6244);
#674=PLANE('',#6252);
#675=PLANE('',#6253);
#676=PLANE('',#6254);
#677=PLANE('',#6256);
#678=PLANE('',#6257);
#679=PLANE('',#6258);
#680=PLANE('',#6259);
#681=PLANE('',#6260);
#682=PLANE('',#6261);
#683=PLANE('',#6262);
#684=PLANE('',#6263);
#685=PLANE('',#6271);
#686=PLANE('',#6286);
#687=PLANE('',#6287);
#688=PLANE('',#6293);
#689=PLANE('',#6300);
#690=PLANE('',#6301);
#691=PLANE('',#6305);
#692=PLANE('',#6307);
#693=PLANE('',#6308);
#694=PLANE('',#6310);
#695=PLANE('',#6316);
#696=PLANE('',#6321);
#697=PLANE('',#6325);
#698=PLANE('',#6326);
#699=PLANE('',#6334);
#700=PLANE('',#6335);
#701=PLANE('',#6337);
#702=PLANE('',#6341);
#703=PLANE('',#6348);
#704=PLANE('',#6349);
#705=PLANE('',#6351);
#706=PLANE('',#6359);
#707=PLANE('',#6367);
#708=PLANE('',#6368);
#709=PLANE('',#6369);
#710=PLANE('',#6370);
#711=PLANE('',#6371);
#712=PLANE('',#6372);
#713=PLANE('',#6373);
#714=PLANE('',#6374);
#715=PLANE('',#6375);
#716=PLANE('',#6377);
#717=PLANE('',#6379);
#718=PLANE('',#6380);
#719=PLANE('',#6381);
#720=PLANE('',#6382);
#721=PLANE('',#6383);
#722=PLANE('',#6384);
#723=PLANE('',#6385);
#724=PLANE('',#6386);
#725=PLANE('',#6395);
#726=PLANE('',#6396);
#727=PLANE('',#6399);
#728=PLANE('',#6407);
#729=PLANE('',#6408);
#730=PLANE('',#6416);
#731=PLANE('',#6417);
#732=PLANE('',#6429);
#733=PLANE('',#6430);
#734=PLANE('',#6432);
#735=PLANE('',#6435);
#736=PLANE('',#6443);
#737=PLANE('',#6444);
#738=PLANE('',#6453);
#739=PLANE('',#6454);
#740=PLANE('',#6457);
#741=PLANE('',#6465);
#742=PLANE('',#6466);
#743=PLANE('',#6474);
#744=PLANE('',#6475);
#745=PLANE('',#6480);
#746=PLANE('',#6496);
#747=PLANE('',#6497);
#748=PLANE('',#6498);
#749=PLANE('',#6499);
#750=PLANE('',#6500);
#751=PLANE('',#6501);
#752=PLANE('',#6504);
#753=PLANE('',#6506);
#754=PLANE('',#6507);
#755=PLANE('',#6509);
#756=PLANE('',#6510);
#757=PLANE('',#6511);
#758=PLANE('',#6516);
#759=PLANE('',#6520);
#760=PLANE('',#6524);
#761=PLANE('',#6528);
#762=PLANE('',#6532);
#763=PLANE('',#6536);
#764=PLANE('',#6539);
#765=PLANE('',#6540);
#766=PLANE('',#6543);
#767=PLANE('',#6544);
#768=PLANE('',#6549);
#769=PLANE('',#6570);
#770=PLANE('',#6571);
#771=PLANE('',#6572);
#772=PLANE('',#6573);
#773=PLANE('',#6574);
#774=PLANE('',#6575);
#775=PLANE('',#6583);
#776=PLANE('',#6584);
#777=PLANE('',#6592);
#778=PLANE('',#6593);
#779=PLANE('',#6595);
#780=PLANE('',#6596);
#781=PLANE('',#6597);
#782=PLANE('',#6598);
#783=PLANE('',#6599);
#784=PLANE('',#6600);
#785=PLANE('',#6601);
#786=PLANE('',#6602);
#787=PLANE('',#6603);
#788=PLANE('',#6605);
#789=PLANE('',#6613);
#790=FACE_OUTER_BOUND('',#1126,.T.);
#791=FACE_OUTER_BOUND('',#1127,.T.);
#792=FACE_OUTER_BOUND('',#1128,.T.);
#793=FACE_OUTER_BOUND('',#1129,.T.);
#794=FACE_OUTER_BOUND('',#1130,.T.);
#795=FACE_OUTER_BOUND('',#1131,.T.);
#796=FACE_OUTER_BOUND('',#1132,.T.);
#797=FACE_OUTER_BOUND('',#1133,.T.);
#798=FACE_OUTER_BOUND('',#1134,.T.);
#799=FACE_OUTER_BOUND('',#1135,.T.);
#800=FACE_OUTER_BOUND('',#1136,.T.);
#801=FACE_OUTER_BOUND('',#1137,.T.);
#802=FACE_OUTER_BOUND('',#1138,.T.);
#803=FACE_OUTER_BOUND('',#1147,.T.);
#804=FACE_OUTER_BOUND('',#1156,.T.);
#805=FACE_OUTER_BOUND('',#1157,.T.);
#806=FACE_OUTER_BOUND('',#1158,.T.);
#807=FACE_OUTER_BOUND('',#1159,.T.);
#808=FACE_OUTER_BOUND('',#1160,.T.);
#809=FACE_OUTER_BOUND('',#1161,.T.);
#810=FACE_OUTER_BOUND('',#1162,.T.);
#811=FACE_OUTER_BOUND('',#1163,.T.);
#812=FACE_OUTER_BOUND('',#1164,.T.);
#813=FACE_OUTER_BOUND('',#1165,.T.);
#814=FACE_OUTER_BOUND('',#1166,.T.);
#815=FACE_OUTER_BOUND('',#1167,.T.);
#816=FACE_OUTER_BOUND('',#1168,.T.);
#817=FACE_OUTER_BOUND('',#1169,.T.);
#818=FACE_OUTER_BOUND('',#1171,.T.);
#819=FACE_OUTER_BOUND('',#1172,.T.);
#820=FACE_OUTER_BOUND('',#1173,.T.);
#821=FACE_OUTER_BOUND('',#1174,.T.);
#822=FACE_OUTER_BOUND('',#1175,.T.);
#823=FACE_OUTER_BOUND('',#1176,.T.);
#824=FACE_OUTER_BOUND('',#1177,.T.);
#825=FACE_OUTER_BOUND('',#1178,.T.);
#826=FACE_OUTER_BOUND('',#1179,.T.);
#827=FACE_OUTER_BOUND('',#1180,.T.);
#828=FACE_OUTER_BOUND('',#1181,.T.);
#829=FACE_OUTER_BOUND('',#1182,.T.);
#830=FACE_OUTER_BOUND('',#1183,.T.);
#831=FACE_OUTER_BOUND('',#1184,.T.);
#832=FACE_OUTER_BOUND('',#1185,.T.);
#833=FACE_OUTER_BOUND('',#1186,.T.);
#834=FACE_OUTER_BOUND('',#1187,.T.);
#835=FACE_OUTER_BOUND('',#1188,.T.);
#836=FACE_OUTER_BOUND('',#1189,.T.);
#837=FACE_OUTER_BOUND('',#1190,.T.);
#838=FACE_OUTER_BOUND('',#1191,.T.);
#839=FACE_OUTER_BOUND('',#1197,.T.);
#840=FACE_OUTER_BOUND('',#1198,.T.);
#841=FACE_OUTER_BOUND('',#1199,.T.);
#842=FACE_OUTER_BOUND('',#1200,.T.);
#843=FACE_OUTER_BOUND('',#1201,.T.);
#844=FACE_OUTER_BOUND('',#1202,.T.);
#845=FACE_OUTER_BOUND('',#1204,.T.);
#846=FACE_OUTER_BOUND('',#1206,.T.);
#847=FACE_OUTER_BOUND('',#1208,.T.);
#848=FACE_OUTER_BOUND('',#1214,.T.);
#849=FACE_OUTER_BOUND('',#1220,.T.);
#850=FACE_OUTER_BOUND('',#1221,.T.);
#851=FACE_OUTER_BOUND('',#1223,.T.);
#852=FACE_OUTER_BOUND('',#1224,.T.);
#853=FACE_OUTER_BOUND('',#1226,.T.);
#854=FACE_OUTER_BOUND('',#1227,.T.);
#855=FACE_OUTER_BOUND('',#1229,.T.);
#856=FACE_OUTER_BOUND('',#1230,.T.);
#857=FACE_OUTER_BOUND('',#1232,.T.);
#858=FACE_OUTER_BOUND('',#1233,.T.);
#859=FACE_OUTER_BOUND('',#1234,.T.);
#860=FACE_OUTER_BOUND('',#1235,.T.);
#861=FACE_OUTER_BOUND('',#1236,.T.);
#862=FACE_OUTER_BOUND('',#1237,.T.);
#863=FACE_OUTER_BOUND('',#1239,.T.);
#864=FACE_OUTER_BOUND('',#1240,.T.);
#865=FACE_OUTER_BOUND('',#1241,.T.);
#866=FACE_OUTER_BOUND('',#1247,.T.);
#867=FACE_OUTER_BOUND('',#1253,.T.);
#868=FACE_OUTER_BOUND('',#1254,.T.);
#869=FACE_OUTER_BOUND('',#1255,.T.);
#870=FACE_OUTER_BOUND('',#1256,.T.);
#871=FACE_OUTER_BOUND('',#1257,.T.);
#872=FACE_OUTER_BOUND('',#1259,.T.);
#873=FACE_OUTER_BOUND('',#1260,.T.);
#874=FACE_OUTER_BOUND('',#1262,.T.);
#875=FACE_OUTER_BOUND('',#1263,.T.);
#876=FACE_OUTER_BOUND('',#1264,.T.);
#877=FACE_OUTER_BOUND('',#1265,.T.);
#878=FACE_OUTER_BOUND('',#1267,.T.);
#879=FACE_OUTER_BOUND('',#1268,.T.);
#880=FACE_OUTER_BOUND('',#1269,.T.);
#881=FACE_OUTER_BOUND('',#1270,.T.);
#882=FACE_OUTER_BOUND('',#1272,.T.);
#883=FACE_OUTER_BOUND('',#1273,.T.);
#884=FACE_OUTER_BOUND('',#1274,.T.);
#885=FACE_OUTER_BOUND('',#1275,.T.);
#886=FACE_OUTER_BOUND('',#1276,.T.);
#887=FACE_OUTER_BOUND('',#1277,.T.);
#888=FACE_OUTER_BOUND('',#1278,.T.);
#889=FACE_OUTER_BOUND('',#1279,.T.);
#890=FACE_OUTER_BOUND('',#1280,.T.);
#891=FACE_OUTER_BOUND('',#1281,.T.);
#892=FACE_OUTER_BOUND('',#1282,.T.);
#893=FACE_OUTER_BOUND('',#1283,.T.);
#894=FACE_OUTER_BOUND('',#1284,.T.);
#895=FACE_OUTER_BOUND('',#1285,.T.);
#896=FACE_OUTER_BOUND('',#1286,.T.);
#897=FACE_OUTER_BOUND('',#1287,.T.);
#898=FACE_OUTER_BOUND('',#1288,.T.);
#899=FACE_OUTER_BOUND('',#1289,.T.);
#900=FACE_OUTER_BOUND('',#1290,.T.);
#901=FACE_OUTER_BOUND('',#1291,.T.);
#902=FACE_OUTER_BOUND('',#1292,.T.);
#903=FACE_OUTER_BOUND('',#1293,.T.);
#904=FACE_OUTER_BOUND('',#1294,.T.);
#905=FACE_OUTER_BOUND('',#1295,.T.);
#906=FACE_OUTER_BOUND('',#1296,.T.);
#907=FACE_OUTER_BOUND('',#1297,.T.);
#908=FACE_OUTER_BOUND('',#1298,.T.);
#909=FACE_OUTER_BOUND('',#1300,.T.);
#910=FACE_OUTER_BOUND('',#1301,.T.);
#911=FACE_OUTER_BOUND('',#1303,.T.);
#912=FACE_OUTER_BOUND('',#1304,.T.);
#913=FACE_OUTER_BOUND('',#1306,.T.);
#914=FACE_OUTER_BOUND('',#1307,.T.);
#915=FACE_OUTER_BOUND('',#1309,.T.);
#916=FACE_OUTER_BOUND('',#1310,.T.);
#917=FACE_OUTER_BOUND('',#1312,.T.);
#918=FACE_OUTER_BOUND('',#1313,.T.);
#919=FACE_OUTER_BOUND('',#1314,.T.);
#920=FACE_OUTER_BOUND('',#1315,.T.);
#921=FACE_OUTER_BOUND('',#1316,.T.);
#922=FACE_OUTER_BOUND('',#1317,.T.);
#923=FACE_OUTER_BOUND('',#1318,.T.);
#924=FACE_OUTER_BOUND('',#1319,.T.);
#925=FACE_OUTER_BOUND('',#1320,.T.);
#926=FACE_OUTER_BOUND('',#1321,.T.);
#927=FACE_OUTER_BOUND('',#1322,.T.);
#928=FACE_OUTER_BOUND('',#1323,.T.);
#929=FACE_OUTER_BOUND('',#1325,.T.);
#930=FACE_OUTER_BOUND('',#1326,.T.);
#931=FACE_OUTER_BOUND('',#1328,.T.);
#932=FACE_OUTER_BOUND('',#1332,.T.);
#933=FACE_OUTER_BOUND('',#1333,.T.);
#934=FACE_OUTER_BOUND('',#1334,.T.);
#935=FACE_OUTER_BOUND('',#1335,.T.);
#936=FACE_OUTER_BOUND('',#1337,.T.);
#937=FACE_OUTER_BOUND('',#1339,.T.);
#938=FACE_OUTER_BOUND('',#1342,.T.);
#939=FACE_OUTER_BOUND('',#1343,.T.);
#940=FACE_OUTER_BOUND('',#1344,.T.);
#941=FACE_OUTER_BOUND('',#1345,.T.);
#942=FACE_OUTER_BOUND('',#1346,.T.);
#943=FACE_OUTER_BOUND('',#1347,.T.);
#944=FACE_OUTER_BOUND('',#1348,.T.);
#945=FACE_OUTER_BOUND('',#1349,.T.);
#946=FACE_OUTER_BOUND('',#1351,.T.);
#947=FACE_OUTER_BOUND('',#1352,.T.);
#948=FACE_OUTER_BOUND('',#1353,.T.);
#949=FACE_OUTER_BOUND('',#1354,.T.);
#950=FACE_OUTER_BOUND('',#1355,.T.);
#951=FACE_OUTER_BOUND('',#1356,.T.);
#952=FACE_OUTER_BOUND('',#1357,.T.);
#953=FACE_OUTER_BOUND('',#1358,.T.);
#954=FACE_OUTER_BOUND('',#1359,.T.);
#955=FACE_OUTER_BOUND('',#1360,.T.);
#956=FACE_OUTER_BOUND('',#1364,.T.);
#957=FACE_OUTER_BOUND('',#1365,.T.);
#958=FACE_OUTER_BOUND('',#1366,.T.);
#959=FACE_OUTER_BOUND('',#1367,.T.);
#960=FACE_OUTER_BOUND('',#1368,.T.);
#961=FACE_OUTER_BOUND('',#1369,.T.);
#962=FACE_OUTER_BOUND('',#1374,.T.);
#963=FACE_OUTER_BOUND('',#1375,.T.);
#964=FACE_OUTER_BOUND('',#1376,.T.);
#965=FACE_OUTER_BOUND('',#1377,.T.);
#966=FACE_OUTER_BOUND('',#1378,.T.);
#967=FACE_OUTER_BOUND('',#1379,.T.);
#968=FACE_OUTER_BOUND('',#1381,.T.);
#969=FACE_OUTER_BOUND('',#1382,.T.);
#970=FACE_OUTER_BOUND('',#1383,.T.);
#971=FACE_OUTER_BOUND('',#1384,.T.);
#972=FACE_OUTER_BOUND('',#1385,.T.);
#973=FACE_OUTER_BOUND('',#1386,.T.);
#974=FACE_OUTER_BOUND('',#1387,.T.);
#975=FACE_OUTER_BOUND('',#1388,.T.);
#976=FACE_OUTER_BOUND('',#1390,.T.);
#977=FACE_OUTER_BOUND('',#1391,.T.);
#978=FACE_OUTER_BOUND('',#1392,.T.);
#979=FACE_OUTER_BOUND('',#1394,.T.);
#980=FACE_OUTER_BOUND('',#1396,.T.);
#981=FACE_OUTER_BOUND('',#1397,.T.);
#982=FACE_OUTER_BOUND('',#1398,.T.);
#983=FACE_OUTER_BOUND('',#1399,.T.);
#984=FACE_OUTER_BOUND('',#1401,.T.);
#985=FACE_OUTER_BOUND('',#1403,.T.);
#986=FACE_OUTER_BOUND('',#1405,.T.);
#987=FACE_OUTER_BOUND('',#1407,.T.);
#988=FACE_OUTER_BOUND('',#1408,.T.);
#989=FACE_OUTER_BOUND('',#1409,.T.);
#990=FACE_OUTER_BOUND('',#1410,.T.);
#991=FACE_OUTER_BOUND('',#1411,.T.);
#992=FACE_OUTER_BOUND('',#1413,.T.);
#993=FACE_OUTER_BOUND('',#1414,.T.);
#994=FACE_OUTER_BOUND('',#1415,.T.);
#995=FACE_OUTER_BOUND('',#1416,.T.);
#996=FACE_OUTER_BOUND('',#1417,.T.);
#997=FACE_OUTER_BOUND('',#1418,.T.);
#998=FACE_OUTER_BOUND('',#1419,.T.);
#999=FACE_OUTER_BOUND('',#1420,.T.);
#1000=FACE_OUTER_BOUND('',#1421,.T.);
#1001=FACE_OUTER_BOUND('',#1422,.T.);
#1002=FACE_OUTER_BOUND('',#1423,.T.);
#1003=FACE_OUTER_BOUND('',#1424,.T.);
#1004=FACE_OUTER_BOUND('',#1425,.T.);
#1005=FACE_OUTER_BOUND('',#1426,.T.);
#1006=FACE_OUTER_BOUND('',#1427,.T.);
#1007=FACE_OUTER_BOUND('',#1428,.T.);
#1008=FACE_OUTER_BOUND('',#1429,.T.);
#1009=FACE_OUTER_BOUND('',#1430,.T.);
#1010=FACE_OUTER_BOUND('',#1431,.T.);
#1011=FACE_OUTER_BOUND('',#1432,.T.);
#1012=FACE_OUTER_BOUND('',#1433,.T.);
#1013=FACE_OUTER_BOUND('',#1435,.T.);
#1014=FACE_OUTER_BOUND('',#1436,.T.);
#1015=FACE_OUTER_BOUND('',#1437,.T.);
#1016=FACE_OUTER_BOUND('',#1438,.T.);
#1017=FACE_OUTER_BOUND('',#1439,.T.);
#1018=FACE_OUTER_BOUND('',#1441,.T.);
#1019=FACE_OUTER_BOUND('',#1443,.T.);
#1020=FACE_OUTER_BOUND('',#1444,.T.);
#1021=FACE_OUTER_BOUND('',#1445,.T.);
#1022=FACE_OUTER_BOUND('',#1446,.T.);
#1023=FACE_OUTER_BOUND('',#1448,.T.);
#1024=FACE_OUTER_BOUND('',#1449,.T.);
#1025=FACE_OUTER_BOUND('',#1450,.T.);
#1026=FACE_OUTER_BOUND('',#1451,.T.);
#1027=FACE_OUTER_BOUND('',#1453,.T.);
#1028=FACE_OUTER_BOUND('',#1455,.T.);
#1029=FACE_OUTER_BOUND('',#1456,.T.);
#1030=FACE_OUTER_BOUND('',#1457,.T.);
#1031=FACE_OUTER_BOUND('',#1458,.T.);
#1032=FACE_OUTER_BOUND('',#1459,.T.);
#1033=FACE_OUTER_BOUND('',#1462,.T.);
#1034=FACE_OUTER_BOUND('',#1463,.T.);
#1035=FACE_OUTER_BOUND('',#1464,.T.);
#1036=FACE_OUTER_BOUND('',#1467,.T.);
#1037=FACE_OUTER_BOUND('',#1468,.T.);
#1038=FACE_OUTER_BOUND('',#1469,.T.);
#1039=FACE_OUTER_BOUND('',#1471,.T.);
#1040=FACE_OUTER_BOUND('',#1473,.T.);
#1041=FACE_OUTER_BOUND('',#1474,.T.);
#1042=FACE_OUTER_BOUND('',#1475,.T.);
#1043=FACE_OUTER_BOUND('',#1477,.T.);
#1044=FACE_OUTER_BOUND('',#1479,.T.);
#1045=FACE_OUTER_BOUND('',#1480,.T.);
#1046=FACE_OUTER_BOUND('',#1481,.T.);
#1047=FACE_OUTER_BOUND('',#1482,.T.);
#1048=FACE_OUTER_BOUND('',#1484,.T.);
#1049=FACE_OUTER_BOUND('',#1485,.T.);
#1050=FACE_OUTER_BOUND('',#1486,.T.);
#1051=FACE_OUTER_BOUND('',#1487,.T.);
#1052=FACE_OUTER_BOUND('',#1489,.T.);
#1053=FACE_OUTER_BOUND('',#1491,.T.);
#1054=FACE_OUTER_BOUND('',#1492,.T.);
#1055=FACE_OUTER_BOUND('',#1493,.T.);
#1056=FACE_OUTER_BOUND('',#1494,.T.);
#1057=FACE_OUTER_BOUND('',#1495,.T.);
#1058=FACE_OUTER_BOUND('',#1496,.T.);
#1059=FACE_OUTER_BOUND('',#1497,.T.);
#1060=FACE_OUTER_BOUND('',#1498,.T.);
#1061=FACE_OUTER_BOUND('',#1499,.T.);
#1062=FACE_OUTER_BOUND('',#1505,.T.);
#1063=FACE_OUTER_BOUND('',#1506,.T.);
#1064=FACE_OUTER_BOUND('',#1512,.T.);
#1065=FACE_OUTER_BOUND('',#1514,.T.);
#1066=FACE_OUTER_BOUND('',#1515,.T.);
#1067=FACE_OUTER_BOUND('',#1516,.T.);
#1068=FACE_OUTER_BOUND('',#1517,.T.);
#1069=FACE_OUTER_BOUND('',#1518,.T.);
#1070=FACE_OUTER_BOUND('',#1519,.T.);
#1071=FACE_OUTER_BOUND('',#1520,.T.);
#1072=FACE_OUTER_BOUND('',#1522,.T.);
#1073=FACE_OUTER_BOUND('',#1523,.T.);
#1074=FACE_OUTER_BOUND('',#1525,.T.);
#1075=FACE_OUTER_BOUND('',#1526,.T.);
#1076=FACE_OUTER_BOUND('',#1528,.T.);
#1077=FACE_OUTER_BOUND('',#1529,.T.);
#1078=FACE_OUTER_BOUND('',#1531,.T.);
#1079=FACE_OUTER_BOUND('',#1532,.T.);
#1080=FACE_OUTER_BOUND('',#1534,.T.);
#1081=FACE_OUTER_BOUND('',#1535,.T.);
#1082=FACE_OUTER_BOUND('',#1537,.T.);
#1083=FACE_OUTER_BOUND('',#1539,.T.);
#1084=FACE_OUTER_BOUND('',#1540,.T.);
#1085=FACE_OUTER_BOUND('',#1541,.T.);
#1086=FACE_OUTER_BOUND('',#1542,.T.);
#1087=FACE_OUTER_BOUND('',#1543,.T.);
#1088=FACE_OUTER_BOUND('',#1545,.T.);
#1089=FACE_OUTER_BOUND('',#1547,.T.);
#1090=FACE_OUTER_BOUND('',#1549,.T.);
#1091=FACE_OUTER_BOUND('',#1551,.T.);
#1092=FACE_OUTER_BOUND('',#1552,.T.);
#1093=FACE_OUTER_BOUND('',#1553,.T.);
#1094=FACE_OUTER_BOUND('',#1554,.T.);
#1095=FACE_OUTER_BOUND('',#1555,.T.);
#1096=FACE_OUTER_BOUND('',#1556,.T.);
#1097=FACE_OUTER_BOUND('',#1557,.T.);
#1098=FACE_OUTER_BOUND('',#1563,.T.);
#1099=FACE_OUTER_BOUND('',#1564,.T.);
#1100=FACE_OUTER_BOUND('',#1570,.T.);
#1101=FACE_OUTER_BOUND('',#1571,.T.);
#1102=FACE_OUTER_BOUND('',#1572,.T.);
#1103=FACE_OUTER_BOUND('',#1573,.T.);
#1104=FACE_OUTER_BOUND('',#1574,.T.);
#1105=FACE_OUTER_BOUND('',#1576,.T.);
#1106=FACE_OUTER_BOUND('',#1578,.T.);
#1107=FACE_OUTER_BOUND('',#1579,.T.);
#1108=FACE_OUTER_BOUND('',#1580,.T.);
#1109=FACE_OUTER_BOUND('',#1582,.T.);
#1110=FACE_OUTER_BOUND('',#1584,.T.);
#1111=FACE_OUTER_BOUND('',#1585,.T.);
#1112=FACE_OUTER_BOUND('',#1586,.T.);
#1113=FACE_OUTER_BOUND('',#1587,.T.);
#1114=FACE_OUTER_BOUND('',#1588,.T.);
#1115=FACE_OUTER_BOUND('',#1589,.T.);
#1116=FACE_OUTER_BOUND('',#1590,.T.);
#1117=FACE_OUTER_BOUND('',#1591,.T.);
#1118=FACE_OUTER_BOUND('',#1592,.T.);
#1119=FACE_OUTER_BOUND('',#1593,.T.);
#1120=FACE_OUTER_BOUND('',#1594,.T.);
#1121=FACE_OUTER_BOUND('',#1595,.T.);
#1122=FACE_OUTER_BOUND('',#1596,.T.);
#1123=FACE_OUTER_BOUND('',#1597,.T.);
#1124=FACE_OUTER_BOUND('',#1599,.T.);
#1125=FACE_OUTER_BOUND('',#1600,.T.);
#1126=EDGE_LOOP('',(#3715,#3716,#3717,#3718));
#1127=EDGE_LOOP('',(#3719,#3720,#3721,#3722));
#1128=EDGE_LOOP('',(#3723,#3724,#3725,#3726));
#1129=EDGE_LOOP('',(#3727,#3728,#3729,#3730));
#1130=EDGE_LOOP('',(#3731,#3732,#3733,#3734));
#1131=EDGE_LOOP('',(#3735,#3736,#3737,#3738));
#1132=EDGE_LOOP('',(#3739,#3740,#3741,#3742));
#1133=EDGE_LOOP('',(#3743,#3744,#3745,#3746));
#1134=EDGE_LOOP('',(#3747,#3748,#3749,#3750));
#1135=EDGE_LOOP('',(#3751,#3752,#3753,#3754));
#1136=EDGE_LOOP('',(#3755,#3756,#3757,#3758));
#1137=EDGE_LOOP('',(#3759,#3760,#3761,#3762));
#1138=EDGE_LOOP('',(#3763,#3764,#3765,#3766));
#1139=EDGE_LOOP('',(#3767));
#1140=EDGE_LOOP('',(#3768));
#1141=EDGE_LOOP('',(#3769));
#1142=EDGE_LOOP('',(#3770));
#1143=EDGE_LOOP('',(#3771));
#1144=EDGE_LOOP('',(#3772));
#1145=EDGE_LOOP('',(#3773));
#1146=EDGE_LOOP('',(#3774));
#1147=EDGE_LOOP('',(#3775,#3776,#3777,#3778));
#1148=EDGE_LOOP('',(#3779));
#1149=EDGE_LOOP('',(#3780));
#1150=EDGE_LOOP('',(#3781));
#1151=EDGE_LOOP('',(#3782));
#1152=EDGE_LOOP('',(#3783));
#1153=EDGE_LOOP('',(#3784));
#1154=EDGE_LOOP('',(#3785));
#1155=EDGE_LOOP('',(#3786));
#1156=EDGE_LOOP('',(#3787,#3788,#3789,#3790));
#1157=EDGE_LOOP('',(#3791,#3792,#3793,#3794));
#1158=EDGE_LOOP('',(#3795,#3796,#3797,#3798));
#1159=EDGE_LOOP('',(#3799,#3800,#3801,#3802));
#1160=EDGE_LOOP('',(#3803,#3804,#3805,#3806));
#1161=EDGE_LOOP('',(#3807,#3808,#3809,#3810));
#1162=EDGE_LOOP('',(#3811,#3812,#3813,#3814,#3815,#3816));
#1163=EDGE_LOOP('',(#3817,#3818,#3819,#3820,#3821,#3822));
#1164=EDGE_LOOP('',(#3823));
#1165=EDGE_LOOP('',(#3824));
#1166=EDGE_LOOP('',(#3825,#3826,#3827,#3828));
#1167=EDGE_LOOP('',(#3829,#3830,#3831,#3832));
#1168=EDGE_LOOP('',(#3833,#3834,#3835,#3836));
#1169=EDGE_LOOP('',(#3837));
#1170=EDGE_LOOP('',(#3838));
#1171=EDGE_LOOP('',(#3839,#3840,#3841,#3842));
#1172=EDGE_LOOP('',(#3843,#3844,#3845,#3846));
#1173=EDGE_LOOP('',(#3847,#3848,#3849,#3850,#3851,#3852));
#1174=EDGE_LOOP('',(#3853,#3854,#3855,#3856));
#1175=EDGE_LOOP('',(#3857));
#1176=EDGE_LOOP('',(#3858,#3859,#3860,#3861));
#1177=EDGE_LOOP('',(#3862));
#1178=EDGE_LOOP('',(#3863,#3864,#3865,#3866));
#1179=EDGE_LOOP('',(#3867));
#1180=EDGE_LOOP('',(#3868,#3869,#3870,#3871));
#1181=EDGE_LOOP('',(#3872));
#1182=EDGE_LOOP('',(#3873,#3874));
#1183=EDGE_LOOP('',(#3875,#3876,#3877,#3878));
#1184=EDGE_LOOP('',(#3879,#3880,#3881,#3882));
#1185=EDGE_LOOP('',(#3883,#3884));
#1186=EDGE_LOOP('',(#3885,#3886,#3887,#3888));
#1187=EDGE_LOOP('',(#3889,#3890));
#1188=EDGE_LOOP('',(#3891,#3892,#3893,#3894));
#1189=EDGE_LOOP('',(#3895,#3896));
#1190=EDGE_LOOP('',(#3897,#3898,#3899,#3900,#3901,#3902,#3903,#3904,#3905,
#3906,#3907,#3908,#3909,#3910,#3911,#3912,#3913,#3914,#3915,#3916));
#1191=EDGE_LOOP('',(#3917));
#1192=EDGE_LOOP('',(#3918,#3919,#3920,#3921,#3922,#3923,#3924,#3925,#3926));
#1193=EDGE_LOOP('',(#3927));
#1194=EDGE_LOOP('',(#3928));
#1195=EDGE_LOOP('',(#3929));
#1196=EDGE_LOOP('',(#3930));
#1197=EDGE_LOOP('',(#3931,#3932,#3933,#3934));
#1198=EDGE_LOOP('',(#3935,#3936,#3937,#3938));
#1199=EDGE_LOOP('',(#3939,#3940,#3941,#3942));
#1200=EDGE_LOOP('',(#3943,#3944,#3945,#3946));
#1201=EDGE_LOOP('',(#3947,#3948,#3949,#3950));
#1202=EDGE_LOOP('',(#3951));
#1203=EDGE_LOOP('',(#3952));
#1204=EDGE_LOOP('',(#3953,#3954,#3955,#3956));
#1205=EDGE_LOOP('',(#3957,#3958));
#1206=EDGE_LOOP('',(#3959,#3960,#3961,#3962));
#1207=EDGE_LOOP('',(#3963,#3964));
#1208=EDGE_LOOP('',(#3965));
#1209=EDGE_LOOP('',(#3966));
#1210=EDGE_LOOP('',(#3967));
#1211=EDGE_LOOP('',(#3968));
#1212=EDGE_LOOP('',(#3969));
#1213=EDGE_LOOP('',(#3970));
#1214=EDGE_LOOP('',(#3971));
#1215=EDGE_LOOP('',(#3972));
#1216=EDGE_LOOP('',(#3973));
#1217=EDGE_LOOP('',(#3974));
#1218=EDGE_LOOP('',(#3975));
#1219=EDGE_LOOP('',(#3976));
#1220=EDGE_LOOP('',(#3977,#3978,#3979,#3980));
#1221=EDGE_LOOP('',(#3981));
#1222=EDGE_LOOP('',(#3982));
#1223=EDGE_LOOP('',(#3983,#3984,#3985,#3986));
#1224=EDGE_LOOP('',(#3987));
#1225=EDGE_LOOP('',(#3988));
#1226=EDGE_LOOP('',(#3989,#3990,#3991,#3992));
#1227=EDGE_LOOP('',(#3993));
#1228=EDGE_LOOP('',(#3994));
#1229=EDGE_LOOP('',(#3995,#3996,#3997,#3998));
#1230=EDGE_LOOP('',(#3999));
#1231=EDGE_LOOP('',(#4000));
#1232=EDGE_LOOP('',(#4001,#4002,#4003,#4004));
#1233=EDGE_LOOP('',(#4005,#4006,#4007,#4008));
#1234=EDGE_LOOP('',(#4009,#4010,#4011,#4012));
#1235=EDGE_LOOP('',(#4013,#4014,#4015,#4016));
#1236=EDGE_LOOP('',(#4017,#4018,#4019,#4020));
#1237=EDGE_LOOP('',(#4021));
#1238=EDGE_LOOP('',(#4022));
#1239=EDGE_LOOP('',(#4023,#4024,#4025,#4026));
#1240=EDGE_LOOP('',(#4027,#4028,#4029,#4030));
#1241=EDGE_LOOP('',(#4031));
#1242=EDGE_LOOP('',(#4032));
#1243=EDGE_LOOP('',(#4033));
#1244=EDGE_LOOP('',(#4034));
#1245=EDGE_LOOP('',(#4035));
#1246=EDGE_LOOP('',(#4036));
#1247=EDGE_LOOP('',(#4037));
#1248=EDGE_LOOP('',(#4038));
#1249=EDGE_LOOP('',(#4039));
#1250=EDGE_LOOP('',(#4040));
#1251=EDGE_LOOP('',(#4041));
#1252=EDGE_LOOP('',(#4042));
#1253=EDGE_LOOP('',(#4043,#4044,#4045,#4046,#4047,#4048));
#1254=EDGE_LOOP('',(#4049,#4050,#4051,#4052,#4053));
#1255=EDGE_LOOP('',(#4054,#4055,#4056,#4057));
#1256=EDGE_LOOP('',(#4058,#4059,#4060,#4061));
#1257=EDGE_LOOP('',(#4062));
#1258=EDGE_LOOP('',(#4063));
#1259=EDGE_LOOP('',(#4064,#4065,#4066,#4067,#4068));
#1260=EDGE_LOOP('',(#4069));
#1261=EDGE_LOOP('',(#4070));
#1262=EDGE_LOOP('',(#4071,#4072,#4073,#4074));
#1263=EDGE_LOOP('',(#4075,#4076,#4077,#4078,#4079,#4080));
#1264=EDGE_LOOP('',(#4081,#4082,#4083,#4084,#4085));
#1265=EDGE_LOOP('',(#4086));
#1266=EDGE_LOOP('',(#4087));
#1267=EDGE_LOOP('',(#4088,#4089,#4090,#4091));
#1268=EDGE_LOOP('',(#4092,#4093,#4094,#4095));
#1269=EDGE_LOOP('',(#4096,#4097,#4098,#4099));
#1270=EDGE_LOOP('',(#4100));
#1271=EDGE_LOOP('',(#4101));
#1272=EDGE_LOOP('',(#4102,#4103,#4104,#4105,#4106));
#1273=EDGE_LOOP('',(#4107,#4108));
#1274=EDGE_LOOP('',(#4109,#4110));
#1275=EDGE_LOOP('',(#4111,#4112));
#1276=EDGE_LOOP('',(#4113,#4114));
#1277=EDGE_LOOP('',(#4115,#4116));
#1278=EDGE_LOOP('',(#4117,#4118));
#1279=EDGE_LOOP('',(#4119,#4120));
#1280=EDGE_LOOP('',(#4121,#4122));
#1281=EDGE_LOOP('',(#4123,#4124,#4125,#4126));
#1282=EDGE_LOOP('',(#4127,#4128,#4129,#4130,#4131,#4132,#4133,#4134,#4135,
#4136,#4137,#4138,#4139,#4140,#4141,#4142,#4143,#4144,#4145,#4146));
#1283=EDGE_LOOP('',(#4147,#4148,#4149,#4150));
#1284=EDGE_LOOP('',(#4151,#4152,#4153,#4154));
#1285=EDGE_LOOP('',(#4155,#4156,#4157,#4158));
#1286=EDGE_LOOP('',(#4159,#4160,#4161,#4162));
#1287=EDGE_LOOP('',(#4163,#4164,#4165,#4166));
#1288=EDGE_LOOP('',(#4167,#4168,#4169,#4170,#4171,#4172));
#1289=EDGE_LOOP('',(#4173,#4174,#4175,#4176));
#1290=EDGE_LOOP('',(#4177,#4178,#4179,#4180));
#1291=EDGE_LOOP('',(#4181,#4182,#4183,#4184));
#1292=EDGE_LOOP('',(#4185,#4186,#4187,#4188));
#1293=EDGE_LOOP('',(#4189,#4190,#4191,#4192));
#1294=EDGE_LOOP('',(#4193,#4194,#4195,#4196));
#1295=EDGE_LOOP('',(#4197,#4198,#4199,#4200,#4201,#4202,#4203,#4204,#4205,
#4206,#4207,#4208,#4209,#4210,#4211,#4212,#4213,#4214,#4215,#4216));
#1296=EDGE_LOOP('',(#4217,#4218,#4219,#4220));
#1297=EDGE_LOOP('',(#4221,#4222,#4223,#4224));
#1298=EDGE_LOOP('',(#4225));
#1299=EDGE_LOOP('',(#4226));
#1300=EDGE_LOOP('',(#4227,#4228,#4229,#4230));
#1301=EDGE_LOOP('',(#4231));
#1302=EDGE_LOOP('',(#4232));
#1303=EDGE_LOOP('',(#4233,#4234,#4235,#4236));
#1304=EDGE_LOOP('',(#4237));
#1305=EDGE_LOOP('',(#4238));
#1306=EDGE_LOOP('',(#4239,#4240,#4241,#4242));
#1307=EDGE_LOOP('',(#4243));
#1308=EDGE_LOOP('',(#4244));
#1309=EDGE_LOOP('',(#4245,#4246,#4247,#4248));
#1310=EDGE_LOOP('',(#4249));
#1311=EDGE_LOOP('',(#4250));
#1312=EDGE_LOOP('',(#4251,#4252,#4253,#4254));
#1313=EDGE_LOOP('',(#4255));
#1314=EDGE_LOOP('',(#4256,#4257,#4258,#4259));
#1315=EDGE_LOOP('',(#4260,#4261,#4262,#4263));
#1316=EDGE_LOOP('',(#4264));
#1317=EDGE_LOOP('',(#4265,#4266,#4267,#4268));
#1318=EDGE_LOOP('',(#4269,#4270,#4271,#4272));
#1319=EDGE_LOOP('',(#4273,#4274));
#1320=EDGE_LOOP('',(#4275,#4276,#4277,#4278,#4279,#4280,#4281,#4282,#4283));
#1321=EDGE_LOOP('',(#4284,#4285));
#1322=EDGE_LOOP('',(#4286,#4287,#4288,#4289));
#1323=EDGE_LOOP('',(#4290));
#1324=EDGE_LOOP('',(#4291));
#1325=EDGE_LOOP('',(#4292,#4293,#4294,#4295));
#1326=EDGE_LOOP('',(#4296));
#1327=EDGE_LOOP('',(#4297));
#1328=EDGE_LOOP('',(#4298,#4299,#4300,#4301));
#1329=EDGE_LOOP('',(#4302));
#1330=EDGE_LOOP('',(#4303));
#1331=EDGE_LOOP('',(#4304));
#1332=EDGE_LOOP('',(#4305,#4306,#4307,#4308));
#1333=EDGE_LOOP('',(#4309,#4310,#4311,#4312));
#1334=EDGE_LOOP('',(#4313,#4314,#4315,#4316,#4317,#4318,#4319,#4320,#4321,
#4322,#4323,#4324));
#1335=EDGE_LOOP('',(#4325,#4326,#4327,#4328));
#1336=EDGE_LOOP('',(#4329));
#1337=EDGE_LOOP('',(#4330,#4331,#4332,#4333));
#1338=EDGE_LOOP('',(#4334));
#1339=EDGE_LOOP('',(#4335,#4336,#4337,#4338));
#1340=EDGE_LOOP('',(#4339));
#1341=EDGE_LOOP('',(#4340));
#1342=EDGE_LOOP('',(#4341,#4342,#4343,#4344));
#1343=EDGE_LOOP('',(#4345,#4346,#4347,#4348));
#1344=EDGE_LOOP('',(#4349,#4350,#4351,#4352));
#1345=EDGE_LOOP('',(#4353,#4354,#4355,#4356));
#1346=EDGE_LOOP('',(#4357,#4358,#4359,#4360));
#1347=EDGE_LOOP('',(#4361,#4362,#4363,#4364));
#1348=EDGE_LOOP('',(#4365,#4366,#4367,#4368,#4369,#4370));
#1349=EDGE_LOOP('',(#4371));
#1350=EDGE_LOOP('',(#4372,#4373,#4374,#4375,#4376,#4377));
#1351=EDGE_LOOP('',(#4378,#4379,#4380,#4381));
#1352=EDGE_LOOP('',(#4382,#4383,#4384,#4385));
#1353=EDGE_LOOP('',(#4386,#4387,#4388,#4389));
#1354=EDGE_LOOP('',(#4390));
#1355=EDGE_LOOP('',(#4391,#4392,#4393,#4394));
#1356=EDGE_LOOP('',(#4395,#4396,#4397,#4398));
#1357=EDGE_LOOP('',(#4399,#4400,#4401,#4402));
#1358=EDGE_LOOP('',(#4403,#4404,#4405,#4406));
#1359=EDGE_LOOP('',(#4407,#4408,#4409,#4410));
#1360=EDGE_LOOP('',(#4411,#4412,#4413,#4414,#4415,#4416,#4417,#4418,#4419,
#4420,#4421,#4422));
#1361=EDGE_LOOP('',(#4423));
#1362=EDGE_LOOP('',(#4424));
#1363=EDGE_LOOP('',(#4425));
#1364=EDGE_LOOP('',(#4426,#4427,#4428,#4429));
#1365=EDGE_LOOP('',(#4430,#4431,#4432,#4433));
#1366=EDGE_LOOP('',(#4434,#4435,#4436,#4437));
#1367=EDGE_LOOP('',(#4438,#4439,#4440,#4441));
#1368=EDGE_LOOP('',(#4442,#4443,#4444,#4445));
#1369=EDGE_LOOP('',(#4446,#4447,#4448,#4449,#4450,#4451,#4452,#4453,#4454,
#4455,#4456,#4457));
#1370=EDGE_LOOP('',(#4458));
#1371=EDGE_LOOP('',(#4459));
#1372=EDGE_LOOP('',(#4460));
#1373=EDGE_LOOP('',(#4461));
#1374=EDGE_LOOP('',(#4462,#4463,#4464,#4465));
#1375=EDGE_LOOP('',(#4466,#4467,#4468,#4469));
#1376=EDGE_LOOP('',(#4470,#4471,#4472,#4473));
#1377=EDGE_LOOP('',(#4474,#4475,#4476,#4477));
#1378=EDGE_LOOP('',(#4478,#4479,#4480,#4481));
#1379=EDGE_LOOP('',(#4482));
#1380=EDGE_LOOP('',(#4483));
#1381=EDGE_LOOP('',(#4484,#4485,#4486,#4487));
#1382=EDGE_LOOP('',(#4488,#4489,#4490,#4491));
#1383=EDGE_LOOP('',(#4492));
#1384=EDGE_LOOP('',(#4493,#4494,#4495,#4496));
#1385=EDGE_LOOP('',(#4497));
#1386=EDGE_LOOP('',(#4498,#4499,#4500,#4501));
#1387=EDGE_LOOP('',(#4502));
#1388=EDGE_LOOP('',(#4503));
#1389=EDGE_LOOP('',(#4504));
#1390=EDGE_LOOP('',(#4505,#4506,#4507,#4508));
#1391=EDGE_LOOP('',(#4509,#4510,#4511,#4512));
#1392=EDGE_LOOP('',(#4513));
#1393=EDGE_LOOP('',(#4514));
#1394=EDGE_LOOP('',(#4515));
#1395=EDGE_LOOP('',(#4516));
#1396=EDGE_LOOP('',(#4517,#4518));
#1397=EDGE_LOOP('',(#4519,#4520,#4521,#4522,#4523,#4524,#4525,#4526,#4527));
#1398=EDGE_LOOP('',(#4528,#4529));
#1399=EDGE_LOOP('',(#4530,#4531,#4532,#4533));
#1400=EDGE_LOOP('',(#4534,#4535,#4536,#4537,#4538));
#1401=EDGE_LOOP('',(#4539,#4540,#4541,#4542));
#1402=EDGE_LOOP('',(#4543,#4544));
#1403=EDGE_LOOP('',(#4545));
#1404=EDGE_LOOP('',(#4546));
#1405=EDGE_LOOP('',(#4547));
#1406=EDGE_LOOP('',(#4548));
#1407=EDGE_LOOP('',(#4549));
#1408=EDGE_LOOP('',(#4550,#4551,#4552,#4553));
#1409=EDGE_LOOP('',(#4554,#4555,#4556,#4557));
#1410=EDGE_LOOP('',(#4558,#4559,#4560,#4561));
#1411=EDGE_LOOP('',(#4562));
#1412=EDGE_LOOP('',(#4563));
#1413=EDGE_LOOP('',(#4564,#4565,#4566,#4567));
#1414=EDGE_LOOP('',(#4568,#4569,#4570,#4571));
#1415=EDGE_LOOP('',(#4572,#4573,#4574,#4575));
#1416=EDGE_LOOP('',(#4576));
#1417=EDGE_LOOP('',(#4577,#4578,#4579,#4580));
#1418=EDGE_LOOP('',(#4581,#4582,#4583,#4584));
#1419=EDGE_LOOP('',(#4585,#4586,#4587,#4588));
#1420=EDGE_LOOP('',(#4589,#4590,#4591,#4592));
#1421=EDGE_LOOP('',(#4593,#4594,#4595,#4596));
#1422=EDGE_LOOP('',(#4597,#4598,#4599,#4600));
#1423=EDGE_LOOP('',(#4601,#4602,#4603,#4604,#4605,#4606));
#1424=EDGE_LOOP('',(#4607,#4608,#4609,#4610,#4611,#4612));
#1425=EDGE_LOOP('',(#4613));
#1426=EDGE_LOOP('',(#4614,#4615,#4616,#4617));
#1427=EDGE_LOOP('',(#4618,#4619,#4620,#4621));
#1428=EDGE_LOOP('',(#4622,#4623,#4624,#4625));
#1429=EDGE_LOOP('',(#4626,#4627,#4628,#4629));
#1430=EDGE_LOOP('',(#4630,#4631,#4632,#4633));
#1431=EDGE_LOOP('',(#4634,#4635,#4636,#4637));
#1432=EDGE_LOOP('',(#4638,#4639,#4640,#4641,#4642,#4643));
#1433=EDGE_LOOP('',(#4644));
#1434=EDGE_LOOP('',(#4645,#4646,#4647,#4648,#4649,#4650));
#1435=EDGE_LOOP('',(#4651,#4652,#4653,#4654));
#1436=EDGE_LOOP('',(#4655,#4656,#4657,#4658));
#1437=EDGE_LOOP('',(#4659,#4660,#4661,#4662));
#1438=EDGE_LOOP('',(#4663));
#1439=EDGE_LOOP('',(#4664));
#1440=EDGE_LOOP('',(#4665));
#1441=EDGE_LOOP('',(#4666));
#1442=EDGE_LOOP('',(#4667));
#1443=EDGE_LOOP('',(#4668,#4669,#4670,#4671));
#1444=EDGE_LOOP('',(#4672,#4673,#4674,#4675));
#1445=EDGE_LOOP('',(#4676,#4677,#4678,#4679));
#1446=EDGE_LOOP('',(#4680));
#1447=EDGE_LOOP('',(#4681));
#1448=EDGE_LOOP('',(#4682));
#1449=EDGE_LOOP('',(#4683,#4684,#4685,#4686));
#1450=EDGE_LOOP('',(#4687,#4688,#4689,#4690));
#1451=EDGE_LOOP('',(#4691));
#1452=EDGE_LOOP('',(#4692));
#1453=EDGE_LOOP('',(#4693));
#1454=EDGE_LOOP('',(#4694));
#1455=EDGE_LOOP('',(#4695,#4696,#4697,#4698));
#1456=EDGE_LOOP('',(#4699,#4700,#4701,#4702));
#1457=EDGE_LOOP('',(#4703,#4704,#4705,#4706));
#1458=EDGE_LOOP('',(#4707,#4708,#4709,#4710));
#1459=EDGE_LOOP('',(#4711,#4712,#4713,#4714));
#1460=EDGE_LOOP('',(#4715));
#1461=EDGE_LOOP('',(#4716));
#1462=EDGE_LOOP('',(#4717,#4718,#4719,#4720));
#1463=EDGE_LOOP('',(#4721,#4722,#4723,#4724));
#1464=EDGE_LOOP('',(#4725,#4726,#4727,#4728));
#1465=EDGE_LOOP('',(#4729));
#1466=EDGE_LOOP('',(#4730));
#1467=EDGE_LOOP('',(#4731,#4732,#4733,#4734));
#1468=EDGE_LOOP('',(#4735,#4736,#4737,#4738));
#1469=EDGE_LOOP('',(#4739));
#1470=EDGE_LOOP('',(#4740));
#1471=EDGE_LOOP('',(#4741));
#1472=EDGE_LOOP('',(#4742));
#1473=EDGE_LOOP('',(#4743,#4744,#4745,#4746));
#1474=EDGE_LOOP('',(#4747));
#1475=EDGE_LOOP('',(#4748));
#1476=EDGE_LOOP('',(#4749));
#1477=EDGE_LOOP('',(#4750));
#1478=EDGE_LOOP('',(#4751));
#1479=EDGE_LOOP('',(#4752,#4753,#4754,#4755));
#1480=EDGE_LOOP('',(#4756,#4757,#4758,#4759));
#1481=EDGE_LOOP('',(#4760,#4761,#4762,#4763));
#1482=EDGE_LOOP('',(#4764));
#1483=EDGE_LOOP('',(#4765));
#1484=EDGE_LOOP('',(#4766));
#1485=EDGE_LOOP('',(#4767,#4768,#4769,#4770));
#1486=EDGE_LOOP('',(#4771,#4772,#4773,#4774));
#1487=EDGE_LOOP('',(#4775));
#1488=EDGE_LOOP('',(#4776));
#1489=EDGE_LOOP('',(#4777));
#1490=EDGE_LOOP('',(#4778));
#1491=EDGE_LOOP('',(#4779,#4780,#4781,#4782));
#1492=EDGE_LOOP('',(#4783));
#1493=EDGE_LOOP('',(#4784,#4785,#4786,#4787));
#1494=EDGE_LOOP('',(#4788,#4789,#4790,#4791));
#1495=EDGE_LOOP('',(#4792,#4793,#4794,#4795));
#1496=EDGE_LOOP('',(#4796,#4797,#4798,#4799));
#1497=EDGE_LOOP('',(#4800,#4801,#4802,#4803));
#1498=EDGE_LOOP('',(#4804,#4805,#4806,#4807));
#1499=EDGE_LOOP('',(#4808,#4809,#4810,#4811));
#1500=EDGE_LOOP('',(#4812));
#1501=EDGE_LOOP('',(#4813));
#1502=EDGE_LOOP('',(#4814));
#1503=EDGE_LOOP('',(#4815));
#1504=EDGE_LOOP('',(#4816));
#1505=EDGE_LOOP('',(#4817,#4818,#4819,#4820));
#1506=EDGE_LOOP('',(#4821,#4822,#4823,#4824));
#1507=EDGE_LOOP('',(#4825));
#1508=EDGE_LOOP('',(#4826));
#1509=EDGE_LOOP('',(#4827));
#1510=EDGE_LOOP('',(#4828));
#1511=EDGE_LOOP('',(#4829));
#1512=EDGE_LOOP('',(#4830,#4831,#4832,#4833));
#1513=EDGE_LOOP('',(#4834));
#1514=EDGE_LOOP('',(#4835,#4836,#4837,#4838));
#1515=EDGE_LOOP('',(#4839,#4840,#4841,#4842));
#1516=EDGE_LOOP('',(#4843,#4844,#4845,#4846));
#1517=EDGE_LOOP('',(#4847,#4848,#4849,#4850));
#1518=EDGE_LOOP('',(#4851,#4852,#4853,#4854));
#1519=EDGE_LOOP('',(#4855,#4856,#4857,#4858));
#1520=EDGE_LOOP('',(#4859));
#1521=EDGE_LOOP('',(#4860));
#1522=EDGE_LOOP('',(#4861,#4862,#4863,#4864));
#1523=EDGE_LOOP('',(#4865));
#1524=EDGE_LOOP('',(#4866));
#1525=EDGE_LOOP('',(#4867,#4868,#4869,#4870));
#1526=EDGE_LOOP('',(#4871));
#1527=EDGE_LOOP('',(#4872));
#1528=EDGE_LOOP('',(#4873,#4874,#4875,#4876));
#1529=EDGE_LOOP('',(#4877));
#1530=EDGE_LOOP('',(#4878));
#1531=EDGE_LOOP('',(#4879,#4880,#4881,#4882));
#1532=EDGE_LOOP('',(#4883));
#1533=EDGE_LOOP('',(#4884));
#1534=EDGE_LOOP('',(#4885,#4886,#4887,#4888));
#1535=EDGE_LOOP('',(#4889));
#1536=EDGE_LOOP('',(#4890));
#1537=EDGE_LOOP('',(#4891,#4892,#4893,#4894));
#1538=EDGE_LOOP('',(#4895,#4896,#4897,#4898));
#1539=EDGE_LOOP('',(#4899,#4900,#4901,#4902));
#1540=EDGE_LOOP('',(#4903,#4904,#4905,#4906));
#1541=EDGE_LOOP('',(#4907,#4908,#4909,#4910));
#1542=EDGE_LOOP('',(#4911,#4912,#4913,#4914));
#1543=EDGE_LOOP('',(#4915));
#1544=EDGE_LOOP('',(#4916));
#1545=EDGE_LOOP('',(#4917,#4918,#4919,#4920));
#1546=EDGE_LOOP('',(#4921,#4922,#4923,#4924));
#1547=EDGE_LOOP('',(#4925));
#1548=EDGE_LOOP('',(#4926));
#1549=EDGE_LOOP('',(#4927,#4928,#4929,#4930));
#1550=EDGE_LOOP('',(#4931,#4932,#4933,#4934));
#1551=EDGE_LOOP('',(#4935,#4936,#4937,#4938));
#1552=EDGE_LOOP('',(#4939,#4940,#4941,#4942));
#1553=EDGE_LOOP('',(#4943,#4944,#4945,#4946));
#1554=EDGE_LOOP('',(#4947,#4948,#4949,#4950));
#1555=EDGE_LOOP('',(#4951,#4952,#4953,#4954));
#1556=EDGE_LOOP('',(#4955,#4956,#4957,#4958));
#1557=EDGE_LOOP('',(#4959,#4960,#4961,#4962));
#1558=EDGE_LOOP('',(#4963));
#1559=EDGE_LOOP('',(#4964));
#1560=EDGE_LOOP('',(#4965));
#1561=EDGE_LOOP('',(#4966));
#1562=EDGE_LOOP('',(#4967));
#1563=EDGE_LOOP('',(#4968,#4969,#4970,#4971));
#1564=EDGE_LOOP('',(#4972,#4973,#4974,#4975));
#1565=EDGE_LOOP('',(#4976));
#1566=EDGE_LOOP('',(#4977));
#1567=EDGE_LOOP('',(#4978));
#1568=EDGE_LOOP('',(#4979));
#1569=EDGE_LOOP('',(#4980));
#1570=EDGE_LOOP('',(#4981,#4982,#4983,#4984));
#1571=EDGE_LOOP('',(#4985,#4986,#4987,#4988));
#1572=EDGE_LOOP('',(#4989,#4990,#4991,#4992));
#1573=EDGE_LOOP('',(#4993,#4994,#4995,#4996));
#1574=EDGE_LOOP('',(#4997));
#1575=EDGE_LOOP('',(#4998));
#1576=EDGE_LOOP('',(#4999));
#1577=EDGE_LOOP('',(#5000));
#1578=EDGE_LOOP('',(#5001,#5002,#5003,#5004));
#1579=EDGE_LOOP('',(#5005,#5006,#5007,#5008));
#1580=EDGE_LOOP('',(#5009));
#1581=EDGE_LOOP('',(#5010));
#1582=EDGE_LOOP('',(#5011));
#1583=EDGE_LOOP('',(#5012));
#1584=EDGE_LOOP('',(#5013,#5014,#5015,#5016));
#1585=EDGE_LOOP('',(#5017,#5018,#5019,#5020));
#1586=EDGE_LOOP('',(#5021,#5022,#5023,#5024));
#1587=EDGE_LOOP('',(#5025,#5026,#5027,#5028));
#1588=EDGE_LOOP('',(#5029,#5030,#5031,#5032));
#1589=EDGE_LOOP('',(#5033,#5034,#5035,#5036));
#1590=EDGE_LOOP('',(#5037,#5038,#5039,#5040,#5041,#5042));
#1591=EDGE_LOOP('',(#5043,#5044,#5045,#5046,#5047,#5048));
#1592=EDGE_LOOP('',(#5049));
#1593=EDGE_LOOP('',(#5050));
#1594=EDGE_LOOP('',(#5051,#5052,#5053,#5054));
#1595=EDGE_LOOP('',(#5055,#5056,#5057,#5058));
#1596=EDGE_LOOP('',(#5059,#5060,#5061,#5062));
#1597=EDGE_LOOP('',(#5063));
#1598=EDGE_LOOP('',(#5064));
#1599=EDGE_LOOP('',(#5065,#5066,#5067,#5068));
#1600=EDGE_LOOP('',(#5069,#5070,#5071,#5072));
#1601=LINE('',#8519,#1930);
#1602=LINE('',#8525,#1931);
#1603=LINE('',#8531,#1932);
#1604=LINE('',#8537,#1933);
#1605=LINE('',#8543,#1934);
#1606=LINE('',#8549,#1935);
#1607=LINE('',#8555,#1936);
#1608=LINE('',#8561,#1937);
#1609=LINE('',#8566,#1938);
#1610=LINE('',#8568,#1939);
#1611=LINE('',#8570,#1940);
#1612=LINE('',#8571,#1941);
#1613=LINE('',#8574,#1942);
#1614=LINE('',#8576,#1943);
#1615=LINE('',#8577,#1944);
#1616=LINE('',#8580,#1945);
#1617=LINE('',#8582,#1946);
#1618=LINE('',#8583,#1947);
#1619=LINE('',#8585,#1948);
#1620=LINE('',#8586,#1949);
#1621=LINE('',#8593,#1950);
#1622=LINE('',#8595,#1951);
#1623=LINE('',#8597,#1952);
#1624=LINE('',#8598,#1953);
#1625=LINE('',#8601,#1954);
#1626=LINE('',#8603,#1955);
#1627=LINE('',#8604,#1956);
#1628=LINE('',#8607,#1957);
#1629=LINE('',#8609,#1958);
#1630=LINE('',#8610,#1959);
#1631=LINE('',#8613,#1960);
#1632=LINE('',#8615,#1961);
#1633=LINE('',#8616,#1962);
#1634=LINE('',#8619,#1963);
#1635=LINE('',#8621,#1964);
#1636=LINE('',#8622,#1965);
#1637=LINE('',#8624,#1966);
#1638=LINE('',#8625,#1967);
#1639=LINE('',#8637,#1968);
#1640=LINE('',#8641,#1969);
#1641=LINE('',#8645,#1970);
#1642=LINE('',#8652,#1971);
#1643=LINE('',#8654,#1972);
#1644=LINE('',#8696,#1973);
#1645=LINE('',#8738,#1974);
#1646=LINE('',#8745,#1975);
#1647=LINE('',#8752,#1976);
#1648=LINE('',#8759,#1977);
#1649=LINE('',#8769,#1978);
#1650=LINE('',#8772,#1979);
#1651=LINE('',#8776,#1980);
#1652=LINE('',#8780,#1981);
#1653=LINE('',#8787,#1982);
#1654=LINE('',#8791,#1983);
#1655=LINE('',#8798,#1984);
#1656=LINE('',#8802,#1985);
#1657=LINE('',#8810,#1986);
#1658=LINE('',#8830,#1987);
#1659=LINE('',#8834,#1988);
#1660=LINE('',#8838,#1989);
#1661=LINE('',#8842,#1990);
#1662=LINE('',#8847,#1991);
#1663=LINE('',#8854,#1992);
#1664=LINE('',#8858,#1993);
#1665=LINE('',#8867,#1994);
#1666=LINE('',#8876,#1995);
#1667=LINE('',#8885,#1996);
#1668=LINE('',#8894,#1997);
#1669=LINE('',#8902,#1998);
#1670=LINE('',#8906,#1999);
#1671=LINE('',#8910,#2000);
#1672=LINE('',#8914,#2001);
#1673=LINE('',#8919,#2002);
#1674=LINE('',#8927,#2003);
#1675=LINE('',#8932,#2004);
#1676=LINE('',#8950,#2005);
#1677=LINE('',#8956,#2006);
#1678=LINE('',#8960,#2007);
#1679=LINE('',#8966,#2008);
#1680=LINE('',#8971,#2009);
#1681=LINE('',#8986,#2010);
#1682=LINE('',#8995,#2011);
#1683=LINE('',#8999,#2012);
#1684=LINE('',#9003,#2013);
#1685=LINE('',#9006,#2014);
#1686=LINE('',#9159,#2015);
#1687=LINE('',#9455,#2016);
#1688=LINE('',#9497,#2017);
#1689=LINE('',#9502,#2018);
#1690=LINE('',#9511,#2019);
#1691=LINE('',#9516,#2020);
#1692=LINE('',#9530,#2021);
#1693=LINE('',#9533,#2022);
#1694=LINE('',#9539,#2023);
#1695=LINE('',#9541,#2024);
#1696=LINE('',#9543,#2025);
#1697=LINE('',#9544,#2026);
#1698=LINE('',#9548,#2027);
#1699=LINE('',#9550,#2028);
#1700=LINE('',#9552,#2029);
#1701=LINE('',#9553,#2030);
#1702=LINE('',#9557,#2031);
#1703=LINE('',#9590,#2032);
#1704=LINE('',#9593,#2033);
#1705=LINE('',#9598,#2034);
#1706=LINE('',#9607,#2035);
#1707=LINE('',#9613,#2036);
#1708=LINE('',#9614,#2037);
#1709=LINE('',#9618,#2038);
#1710=LINE('',#9622,#2039);
#1711=LINE('',#9626,#2040);
#1712=LINE('',#9628,#2041);
#1713=LINE('',#9631,#2042);
#1714=LINE('',#9633,#2043);
#1715=LINE('',#9639,#2044);
#1716=LINE('',#9641,#2045);
#1717=LINE('',#9643,#2046);
#1718=LINE('',#9644,#2047);
#1719=LINE('',#9647,#2048);
#1720=LINE('',#9649,#2049);
#1721=LINE('',#9650,#2050);
#1722=LINE('',#9653,#2051);
#1723=LINE('',#9655,#2052);
#1724=LINE('',#9656,#2053);
#1725=LINE('',#9659,#2054);
#1726=LINE('',#9661,#2055);
#1727=LINE('',#9662,#2056);
#1728=LINE('',#9665,#2057);
#1729=LINE('',#9667,#2058);
#1730=LINE('',#9668,#2059);
#1731=LINE('',#9670,#2060);
#1732=LINE('',#9671,#2061);
#1733=LINE('',#9679,#2062);
#1734=LINE('',#9683,#2063);
#1735=LINE('',#9687,#2064);
#1736=LINE('',#9695,#2065);
#1737=LINE('',#9701,#2066);
#1738=LINE('',#9707,#2067);
#1739=LINE('',#9712,#2068);
#1740=LINE('',#9716,#2069);
#1741=LINE('',#9720,#2070);
#1742=LINE('',#9722,#2071);
#1743=LINE('',#9723,#2072);
#1744=LINE('',#9726,#2073);
#1745=LINE('',#9730,#2074);
#1746=LINE('',#9734,#2075);
#1747=LINE('',#9738,#2076);
#1748=LINE('',#9742,#2077);
#1749=LINE('',#9746,#2078);
#1750=LINE('',#9747,#2079);
#1751=LINE('',#9750,#2080);
#1752=LINE('',#9755,#2081);
#1753=LINE('',#9758,#2082);
#1754=LINE('',#9760,#2083);
#1755=LINE('',#9764,#2084);
#1756=LINE('',#9765,#2085);
#1757=LINE('',#9768,#2086);
#1758=LINE('',#9772,#2087);
#1759=LINE('',#9774,#2088);
#1760=LINE('',#9779,#2089);
#1761=LINE('',#9780,#2090);
#1762=LINE('',#9782,#2091);
#1763=LINE('',#9791,#2092);
#1764=LINE('',#9794,#2093);
#1765=LINE('',#9802,#2094);
#1766=LINE('',#9809,#2095);
#1767=LINE('',#9818,#2096);
#1768=LINE('',#9824,#2097);
#1769=LINE('',#9832,#2098);
#1770=LINE('',#9862,#2099);
#1771=LINE('',#9909,#2100);
#1772=LINE('',#9914,#2101);
#1773=LINE('',#9920,#2102);
#1774=LINE('',#9931,#2103);
#1775=LINE('',#9935,#2104);
#1776=LINE('',#9939,#2105);
#1777=LINE('',#9946,#2106);
#1778=LINE('',#9950,#2107);
#1779=LINE('',#9954,#2108);
#1780=LINE('',#9959,#2109);
#1781=LINE('',#9961,#2110);
#1782=LINE('',#9963,#2111);
#1783=LINE('',#9964,#2112);
#1784=LINE('',#9967,#2113);
#1785=LINE('',#9969,#2114);
#1786=LINE('',#9970,#2115);
#1787=LINE('',#9973,#2116);
#1788=LINE('',#9975,#2117);
#1789=LINE('',#9976,#2118);
#1790=LINE('',#9979,#2119);
#1791=LINE('',#9981,#2120);
#1792=LINE('',#9982,#2121);
#1793=LINE('',#9985,#2122);
#1794=LINE('',#9987,#2123);
#1795=LINE('',#9988,#2124);
#1796=LINE('',#9990,#2125);
#1797=LINE('',#9991,#2126);
#1798=LINE('',#10001,#2127);
#1799=LINE('',#10003,#2128);
#1800=LINE('',#10005,#2129);
#1801=LINE('',#10006,#2130);
#1802=LINE('',#10009,#2131);
#1803=LINE('',#10011,#2132);
#1804=LINE('',#10012,#2133);
#1805=LINE('',#10015,#2134);
#1806=LINE('',#10017,#2135);
#1807=LINE('',#10018,#2136);
#1808=LINE('',#10021,#2137);
#1809=LINE('',#10023,#2138);
#1810=LINE('',#10024,#2139);
#1811=LINE('',#10027,#2140);
#1812=LINE('',#10029,#2141);
#1813=LINE('',#10030,#2142);
#1814=LINE('',#10032,#2143);
#1815=LINE('',#10033,#2144);
#1816=LINE('',#10041,#2145);
#1817=LINE('',#10043,#2146);
#1818=LINE('',#10049,#2147);
#1819=LINE('',#10063,#2148);
#1820=LINE('',#10066,#2149);
#1821=LINE('',#10071,#2150);
#1822=LINE('',#10079,#2151);
#1823=LINE('',#10085,#2152);
#1824=LINE('',#10095,#2153);
#1825=LINE('',#10101,#2154);
#1826=LINE('',#10106,#2155);
#1827=LINE('',#10110,#2156);
#1828=LINE('',#10114,#2157);
#1829=LINE('',#10116,#2158);
#1830=LINE('',#10117,#2159);
#1831=LINE('',#10120,#2160);
#1832=LINE('',#10124,#2161);
#1833=LINE('',#10125,#2162);
#1834=LINE('',#10134,#2163);
#1835=LINE('',#10140,#2164);
#1836=LINE('',#10153,#2165);
#1837=LINE('',#10167,#2166);
#1838=LINE('',#10170,#2167);
#1839=LINE('',#10175,#2168);
#1840=LINE('',#10183,#2169);
#1841=LINE('',#10189,#2170);
#1842=LINE('',#10198,#2171);
#1843=LINE('',#10205,#2172);
#1844=LINE('',#10211,#2173);
#1845=LINE('',#10217,#2174);
#1846=LINE('',#10223,#2175);
#1847=LINE('',#10229,#2176);
#1848=LINE('',#10234,#2177);
#1849=LINE('',#10236,#2178);
#1850=LINE('',#10238,#2179);
#1851=LINE('',#10239,#2180);
#1852=LINE('',#10242,#2181);
#1853=LINE('',#10244,#2182);
#1854=LINE('',#10245,#2183);
#1855=LINE('',#10248,#2184);
#1856=LINE('',#10250,#2185);
#1857=LINE('',#10251,#2186);
#1858=LINE('',#10253,#2187);
#1859=LINE('',#10254,#2188);
#1860=LINE('',#10264,#2189);
#1861=LINE('',#10266,#2190);
#1862=LINE('',#10267,#2191);
#1863=LINE('',#10270,#2192);
#1864=LINE('',#10272,#2193);
#1865=LINE('',#10273,#2194);
#1866=LINE('',#10278,#2195);
#1867=LINE('',#10279,#2196);
#1868=LINE('',#10281,#2197);
#1869=LINE('',#10282,#2198);
#1870=LINE('',#10292,#2199);
#1871=LINE('',#10299,#2200);
#1872=LINE('',#10306,#2201);
#1873=LINE('',#10313,#2202);
#1874=LINE('',#10320,#2203);
#1875=LINE('',#10325,#2204);
#1876=LINE('',#10332,#2205);
#1877=LINE('',#10335,#2206);
#1878=LINE('',#10338,#2207);
#1879=LINE('',#10340,#2208);
#1880=LINE('',#10341,#2209);
#1881=LINE('',#10347,#2210);
#1882=LINE('',#10349,#2211);
#1883=LINE('',#10350,#2212);
#1884=LINE('',#10359,#2213);
#1885=LINE('',#10364,#2214);
#1886=LINE('',#10372,#2215);
#1887=LINE('',#10378,#2216);
#1888=LINE('',#10384,#2217);
#1889=LINE('',#10390,#2218);
#1890=LINE('',#10396,#2219);
#1891=LINE('',#10401,#2220);
#1892=LINE('',#10403,#2221);
#1893=LINE('',#10405,#2222);
#1894=LINE('',#10406,#2223);
#1895=LINE('',#10409,#2224);
#1896=LINE('',#10411,#2225);
#1897=LINE('',#10412,#2226);
#1898=LINE('',#10415,#2227);
#1899=LINE('',#10417,#2228);
#1900=LINE('',#10418,#2229);
#1901=LINE('',#10420,#2230);
#1902=LINE('',#10421,#2231);
#1903=LINE('',#10429,#2232);
#1904=LINE('',#10435,#2233);
#1905=LINE('',#10444,#2234);
#1906=LINE('',#10450,#2235);
#1907=LINE('',#10458,#2236);
#1908=LINE('',#10460,#2237);
#1909=LINE('',#10462,#2238);
#1910=LINE('',#10463,#2239);
#1911=LINE('',#10466,#2240);
#1912=LINE('',#10468,#2241);
#1913=LINE('',#10469,#2242);
#1914=LINE('',#10472,#2243);
#1915=LINE('',#10474,#2244);
#1916=LINE('',#10475,#2245);
#1917=LINE('',#10478,#2246);
#1918=LINE('',#10480,#2247);
#1919=LINE('',#10481,#2248);
#1920=LINE('',#10484,#2249);
#1921=LINE('',#10486,#2250);
#1922=LINE('',#10487,#2251);
#1923=LINE('',#10489,#2252);
#1924=LINE('',#10490,#2253);
#1925=LINE('',#10502,#2254);
#1926=LINE('',#10506,#2255);
#1927=LINE('',#10510,#2256);
#1928=LINE('',#10517,#2257);
#1929=LINE('',#10519,#2258);
#1930=VECTOR('',#6681,0.164999999999999);
#1931=VECTOR('',#6688,0.164999999999999);
#1932=VECTOR('',#6695,0.165);
#1933=VECTOR('',#6702,0.165);
#1934=VECTOR('',#6709,0.21);
#1935=VECTOR('',#6716,0.21);
#1936=VECTOR('',#6723,0.21);
#1937=VECTOR('',#6730,0.21);
#1938=VECTOR('',#6735,1.);
#1939=VECTOR('',#6736,1.);
#1940=VECTOR('',#6737,1.);
#1941=VECTOR('',#6738,1.);
#1942=VECTOR('',#6741,1.);
#1943=VECTOR('',#6742,1.);
#1944=VECTOR('',#6743,1.);
#1945=VECTOR('',#6746,1.);
#1946=VECTOR('',#6747,1.);
#1947=VECTOR('',#6748,1.);
#1948=VECTOR('',#6751,1.);
#1949=VECTOR('',#6752,1.);
#1950=VECTOR('',#6761,1.);
#1951=VECTOR('',#6762,1.);
#1952=VECTOR('',#6763,1.);
#1953=VECTOR('',#6764,1.);
#1954=VECTOR('',#6767,1.);
#1955=VECTOR('',#6768,1.);
#1956=VECTOR('',#6769,1.);
#1957=VECTOR('',#6772,1.);
#1958=VECTOR('',#6773,1.);
#1959=VECTOR('',#6774,1.);
#1960=VECTOR('',#6777,1.);
#1961=VECTOR('',#6778,1.);
#1962=VECTOR('',#6779,1.);
#1963=VECTOR('',#6782,1.);
#1964=VECTOR('',#6783,1.);
#1965=VECTOR('',#6784,1.);
#1966=VECTOR('',#6787,1.);
#1967=VECTOR('',#6788,1.);
#1968=VECTOR('',#6805,0.4);
#1969=VECTOR('',#6810,0.425);
#1970=VECTOR('',#6815,0.41);
#1971=VECTOR('',#6824,0.26);
#1972=VECTOR('',#6827,0.25);
#1973=VECTOR('',#6832,0.25);
#1974=VECTOR('',#6837,0.165);
#1975=VECTOR('',#6846,0.165);
#1976=VECTOR('',#6855,0.165);
#1977=VECTOR('',#6864,0.165);
#1978=VECTOR('',#6877,1.);
#1979=VECTOR('',#6880,1.);
#1980=VECTOR('',#6883,1.);
#1981=VECTOR('',#6886,1.);
#1982=VECTOR('',#6895,1.);
#1983=VECTOR('',#6898,1.);
#1984=VECTOR('',#6907,1.);
#1985=VECTOR('',#6910,1.);
#1986=VECTOR('',#6921,2.2);
#1987=VECTOR('',#6948,0.275);
#1988=VECTOR('',#6953,0.275);
#1989=VECTOR('',#6958,0.275);
#1990=VECTOR('',#6963,0.275);
#1991=VECTOR('',#6968,1.5);
#1992=VECTOR('',#6977,3.);
#1993=VECTOR('',#6982,1.02);
#1994=VECTOR('',#6995,0.375);
#1995=VECTOR('',#7006,0.375);
#1996=VECTOR('',#7017,0.375);
#1997=VECTOR('',#7028,0.375);
#1998=VECTOR('',#7039,0.225);
#1999=VECTOR('',#7044,0.225);
#2000=VECTOR('',#7049,0.225);
#2001=VECTOR('',#7054,0.225);
#2002=VECTOR('',#7059,1.49);
#2003=VECTOR('',#7070,0.71);
#2004=VECTOR('',#7075,2.2);
#2005=VECTOR('',#7100,0.976185);
#2006=VECTOR('',#7107,0.5);
#2007=VECTOR('',#7112,0.53);
#2008=VECTOR('',#7121,0.976185);
#2009=VECTOR('',#7128,0.53);
#2010=VECTOR('',#7147,1.023815);
#2011=VECTOR('',#7158,1.47);
#2012=VECTOR('',#7163,1.5);
#2013=VECTOR('',#7168,1.47);
#2014=VECTOR('',#7173,1.023815);
#2015=VECTOR('',#7224,1.019052);
#2016=VECTOR('',#7301,0.980948);
#2017=VECTOR('',#7330,1.013815);
#2018=VECTOR('',#7337,0.991185);
#2019=VECTOR('',#7348,1.013815);
#2020=VECTOR('',#7355,0.991185);
#2021=VECTOR('',#7376,0.55);
#2022=VECTOR('',#7381,0.6);
#2023=VECTOR('',#7388,1.);
#2024=VECTOR('',#7389,1.);
#2025=VECTOR('',#7390,1.);
#2026=VECTOR('',#7391,1.);
#2027=VECTOR('',#7394,1.);
#2028=VECTOR('',#7395,1.);
#2029=VECTOR('',#7396,1.);
#2030=VECTOR('',#7397,1.);
#2031=VECTOR('',#7400,1.);
#2032=VECTOR('',#7407,0.165);
#2033=VECTOR('',#7412,1.);
#2034=VECTOR('',#7417,0.4);
#2035=VECTOR('',#7428,0.4);
#2036=VECTOR('',#7437,1.);
#2037=VECTOR('',#7438,1.);
#2038=VECTOR('',#7443,0.225);
#2039=VECTOR('',#7448,0.225);
#2040=VECTOR('',#7453,0.6);
#2041=VECTOR('',#7454,0.6);
#2042=VECTOR('',#7459,1.);
#2043=VECTOR('',#7462,1.);
#2044=VECTOR('',#7469,1.);
#2045=VECTOR('',#7470,1.);
#2046=VECTOR('',#7471,1.);
#2047=VECTOR('',#7472,1.);
#2048=VECTOR('',#7475,1.);
#2049=VECTOR('',#7476,1.);
#2050=VECTOR('',#7477,1.);
#2051=VECTOR('',#7480,1.);
#2052=VECTOR('',#7481,1.);
#2053=VECTOR('',#7482,1.);
#2054=VECTOR('',#7485,1.);
#2055=VECTOR('',#7486,1.);
#2056=VECTOR('',#7487,1.);
#2057=VECTOR('',#7490,1.);
#2058=VECTOR('',#7491,1.);
#2059=VECTOR('',#7492,1.);
#2060=VECTOR('',#7495,1.);
#2061=VECTOR('',#7496,1.);
#2062=VECTOR('',#7507,0.185);
#2063=VECTOR('',#7512,0.2);
#2064=VECTOR('',#7517,0.1625);
#2065=VECTOR('',#7528,0.25);
#2066=VECTOR('',#7535,0.25);
#2067=VECTOR('',#7542,0.225);
#2068=VECTOR('',#7547,1.);
#2069=VECTOR('',#7550,1.);
#2070=VECTOR('',#7555,1.);
#2071=VECTOR('',#7556,1.);
#2072=VECTOR('',#7557,1.);
#2073=VECTOR('',#7560,1.);
#2074=VECTOR('',#7563,1.);
#2075=VECTOR('',#7566,1.);
#2076=VECTOR('',#7569,1.);
#2077=VECTOR('',#7572,1.);
#2078=VECTOR('',#7577,1.);
#2079=VECTOR('',#7578,1.);
#2080=VECTOR('',#7581,1.);
#2081=VECTOR('',#7588,1.);
#2082=VECTOR('',#7591,1.);
#2083=VECTOR('',#7592,1.);
#2084=VECTOR('',#7597,1.);
#2085=VECTOR('',#7598,1.);
#2086=VECTOR('',#7601,1.);
#2087=VECTOR('',#7604,1.);
#2088=VECTOR('',#7607,1.);
#2089=VECTOR('',#7614,1.);
#2090=VECTOR('',#7615,1.);
#2091=VECTOR('',#7618,1.);
#2092=VECTOR('',#7631,0.7);
#2093=VECTOR('',#7634,0.5);
#2094=VECTOR('',#7645,0.165);
#2095=VECTOR('',#7654,0.6);
#2096=VECTOR('',#7667,0.505);
#2097=VECTOR('',#7674,0.7);
#2098=VECTOR('',#7685,1.);
#2099=VECTOR('',#7692,0.165);
#2100=VECTOR('',#7695,1.);
#2101=VECTOR('',#7700,0.505);
#2102=VECTOR('',#7707,0.9);
#2103=VECTOR('',#7724,0.325);
#2104=VECTOR('',#7729,0.35);
#2105=VECTOR('',#7734,0.335);
#2106=VECTOR('',#7743,0.21);
#2107=VECTOR('',#7748,0.2);
#2108=VECTOR('',#7753,0.18);
#2109=VECTOR('',#7758,1.);
#2110=VECTOR('',#7759,1.);
#2111=VECTOR('',#7760,1.);
#2112=VECTOR('',#7761,1.);
#2113=VECTOR('',#7764,1.);
#2114=VECTOR('',#7765,1.);
#2115=VECTOR('',#7766,1.);
#2116=VECTOR('',#7769,1.);
#2117=VECTOR('',#7770,1.);
#2118=VECTOR('',#7771,1.);
#2119=VECTOR('',#7774,1.);
#2120=VECTOR('',#7775,1.);
#2121=VECTOR('',#7776,1.);
#2122=VECTOR('',#7779,1.);
#2123=VECTOR('',#7780,1.);
#2124=VECTOR('',#7781,1.);
#2125=VECTOR('',#7784,1.);
#2126=VECTOR('',#7785,1.);
#2127=VECTOR('',#7798,1.);
#2128=VECTOR('',#7799,1.);
#2129=VECTOR('',#7800,1.);
#2130=VECTOR('',#7801,1.);
#2131=VECTOR('',#7804,1.);
#2132=VECTOR('',#7805,1.);
#2133=VECTOR('',#7806,1.);
#2134=VECTOR('',#7809,1.);
#2135=VECTOR('',#7810,1.);
#2136=VECTOR('',#7811,1.);
#2137=VECTOR('',#7814,1.);
#2138=VECTOR('',#7815,1.);
#2139=VECTOR('',#7816,1.);
#2140=VECTOR('',#7819,1.);
#2141=VECTOR('',#7820,1.);
#2142=VECTOR('',#7821,1.);
#2143=VECTOR('',#7824,1.);
#2144=VECTOR('',#7825,1.);
#2145=VECTOR('',#7836,0.185);
#2146=VECTOR('',#7839,0.2);
#2147=VECTOR('',#7846,0.165);
#2148=VECTOR('',#7865,0.7);
#2149=VECTOR('',#7868,0.3);
#2150=VECTOR('',#7875,0.3);
#2151=VECTOR('',#7886,0.305);
#2152=VECTOR('',#7893,0.5);
#2153=VECTOR('',#7908,0.5);
#2154=VECTOR('',#7915,0.5);
#2155=VECTOR('',#7920,1.);
#2156=VECTOR('',#7923,1.);
#2157=VECTOR('',#7928,1.);
#2158=VECTOR('',#7929,1.);
#2159=VECTOR('',#7930,1.);
#2160=VECTOR('',#7933,1.);
#2161=VECTOR('',#7938,1.);
#2162=VECTOR('',#7939,1.);
#2163=VECTOR('',#7952,0.305);
#2164=VECTOR('',#7959,0.5);
#2165=VECTOR('',#7980,0.165);
#2166=VECTOR('',#7999,0.699999999999999);
#2167=VECTOR('',#8002,0.3);
#2168=VECTOR('',#8009,0.3);
#2169=VECTOR('',#8020,0.305);
#2170=VECTOR('',#8027,0.5);
#2171=VECTOR('',#8040,0.25);
#2172=VECTOR('',#8049,0.165);
#2173=VECTOR('',#8056,0.165);
#2174=VECTOR('',#8063,0.165);
#2175=VECTOR('',#8070,0.165);
#2176=VECTOR('',#8077,1.05);
#2177=VECTOR('',#8082,1.);
#2178=VECTOR('',#8083,1.);
#2179=VECTOR('',#8084,1.);
#2180=VECTOR('',#8085,1.);
#2181=VECTOR('',#8088,1.);
#2182=VECTOR('',#8089,1.);
#2183=VECTOR('',#8090,1.);
#2184=VECTOR('',#8093,1.);
#2185=VECTOR('',#8094,1.);
#2186=VECTOR('',#8095,1.);
#2187=VECTOR('',#8098,1.);
#2188=VECTOR('',#8099,1.);
#2189=VECTOR('',#8112,1.);
#2190=VECTOR('',#8113,1.);
#2191=VECTOR('',#8114,1.);
#2192=VECTOR('',#8117,1.);
#2193=VECTOR('',#8118,1.);
#2194=VECTOR('',#8119,1.);
#2195=VECTOR('',#8124,1.);
#2196=VECTOR('',#8125,1.);
#2197=VECTOR('',#8128,1.);
#2198=VECTOR('',#8129,1.);
#2199=VECTOR('',#8142,1.05);
#2200=VECTOR('',#8151,1.);
#2201=VECTOR('',#8160,1.05);
#2202=VECTOR('',#8169,1.);
#2203=VECTOR('',#8178,1.05);
#2204=VECTOR('',#8185,0.9);
#2205=VECTOR('',#8192,1.);
#2206=VECTOR('',#8195,1.);
#2207=VECTOR('',#8198,1.);
#2208=VECTOR('',#8199,1.);
#2209=VECTOR('',#8200,1.);
#2210=VECTOR('',#8207,1.);
#2211=VECTOR('',#8210,1.);
#2212=VECTOR('',#8211,1.);
#2213=VECTOR('',#8222,0.895);
#2214=VECTOR('',#8229,0.605);
#2215=VECTOR('',#8240,0.225);
#2216=VECTOR('',#8247,0.225);
#2217=VECTOR('',#8254,0.225);
#2218=VECTOR('',#8261,0.225);
#2219=VECTOR('',#8268,0.7);
#2220=VECTOR('',#8273,1.);
#2221=VECTOR('',#8274,1.);
#2222=VECTOR('',#8275,1.);
#2223=VECTOR('',#8276,1.);
#2224=VECTOR('',#8279,1.);
#2225=VECTOR('',#8280,1.);
#2226=VECTOR('',#8281,1.);
#2227=VECTOR('',#8284,1.);
#2228=VECTOR('',#8285,1.);
#2229=VECTOR('',#8286,1.);
#2230=VECTOR('',#8289,1.);
#2231=VECTOR('',#8290,1.);
#2232=VECTOR('',#8301,0.305);
#2233=VECTOR('',#8308,0.5);
#2234=VECTOR('',#8321,0.225);
#2235=VECTOR('',#8328,0.5);
#2236=VECTOR('',#8339,1.);
#2237=VECTOR('',#8340,1.);
#2238=VECTOR('',#8341,1.);
#2239=VECTOR('',#8342,1.);
#2240=VECTOR('',#8345,1.);
#2241=VECTOR('',#8346,1.);
#2242=VECTOR('',#8347,1.);
#2243=VECTOR('',#8350,1.);
#2244=VECTOR('',#8351,1.);
#2245=VECTOR('',#8352,1.);
#2246=VECTOR('',#8355,1.);
#2247=VECTOR('',#8356,1.);
#2248=VECTOR('',#8357,1.);
#2249=VECTOR('',#8360,1.);
#2250=VECTOR('',#8361,1.);
#2251=VECTOR('',#8362,1.);
#2252=VECTOR('',#8365,1.);
#2253=VECTOR('',#8366,1.);
#2254=VECTOR('',#8383,0.325);
#2255=VECTOR('',#8388,0.35);
#2256=VECTOR('',#8393,0.335);
#2257=VECTOR('',#8402,0.21);
#2258=VECTOR('',#8405,0.2);
#2259=CIRCLE('',#5919,0.164999999999999);
#2260=CIRCLE('',#5920,0.164999999999999);
#2261=CIRCLE('',#5922,0.164999999999999);
#2262=CIRCLE('',#5923,0.164999999999999);
#2263=CIRCLE('',#5925,0.165);
#2264=CIRCLE('',#5926,0.165);
#2265=CIRCLE('',#5928,0.165);
#2266=CIRCLE('',#5929,0.165);
#2267=CIRCLE('',#5931,0.21);
#2268=CIRCLE('',#5932,0.21);
#2269=CIRCLE('',#5934,0.21);
#2270=CIRCLE('',#5935,0.21);
#2271=CIRCLE('',#5937,0.21);
#2272=CIRCLE('',#5938,0.21);
#2273=CIRCLE('',#5940,0.21);
#2274=CIRCLE('',#5941,0.21);
#2275=CIRCLE('',#5958,0.24505);
#2276=CIRCLE('',#5960,0.375);
#2277=CIRCLE('',#5962,0.425);
#2278=CIRCLE('',#5964,0.425);
#2279=CIRCLE('',#5966,0.395);
#2280=CIRCLE('',#5968,0.27);
#2281=CIRCLE('',#5970,0.24505);
#2282=CIRCLE('',#5975,0.165);
#2283=CIRCLE('',#5976,0.165);
#2284=CIRCLE('',#5979,0.165);
#2285=CIRCLE('',#5980,0.165);
#2286=CIRCLE('',#5983,0.165);
#2287=CIRCLE('',#5984,0.165);
#2288=CIRCLE('',#5987,0.165);
#2289=CIRCLE('',#5988,0.165);
#2290=CIRCLE('',#5991,2.2);
#2291=CIRCLE('',#5992,0.525);
#2292=CIRCLE('',#5994,0.525);
#2293=CIRCLE('',#5996,0.525);
#2294=CIRCLE('',#5997,0.525);
#2295=CIRCLE('',#5999,2.2);
#2296=CIRCLE('',#6001,0.525);
#2297=CIRCLE('',#6002,0.525);
#2298=CIRCLE('',#6004,2.2);
#2299=CIRCLE('',#6006,0.525);
#2300=CIRCLE('',#6007,0.525);
#2301=CIRCLE('',#6009,2.2);
#2302=CIRCLE('',#6011,2.2);
#2303=CIRCLE('',#6012,2.2);
#2304=CIRCLE('',#6013,2.2);
#2305=CIRCLE('',#6014,2.2);
#2306=CIRCLE('',#6015,2.2);
#2307=CIRCLE('',#6016,2.2);
#2308=CIRCLE('',#6018,3.);
#2309=CIRCLE('',#6019,0.275);
#2310=CIRCLE('',#6020,0.275);
#2311=CIRCLE('',#6021,0.275);
#2312=CIRCLE('',#6022,0.275);
#2313=CIRCLE('',#6024,0.275);
#2314=CIRCLE('',#6026,0.275);
#2315=CIRCLE('',#6028,0.275);
#2316=CIRCLE('',#6030,0.275);
#2317=CIRCLE('',#6032,1.5);
#2318=CIRCLE('',#6033,1.5);
#2319=CIRCLE('',#6035,1.02);
#2320=CIRCLE('',#6037,3.);
#2321=CIRCLE('',#6039,1.02);
#2322=CIRCLE('',#6044,0.375);
#2323=CIRCLE('',#6045,0.375);
#2324=CIRCLE('',#6047,0.225);
#2325=CIRCLE('',#6049,0.375);
#2326=CIRCLE('',#6050,0.375);
#2327=CIRCLE('',#6052,0.225);
#2328=CIRCLE('',#6054,0.375);
#2329=CIRCLE('',#6055,0.375);
#2330=CIRCLE('',#6057,0.225);
#2331=CIRCLE('',#6059,0.375);
#2332=CIRCLE('',#6060,0.375);
#2333=CIRCLE('',#6062,0.225);
#2334=CIRCLE('',#6064,0.225);
#2335=CIRCLE('',#6066,0.225);
#2336=CIRCLE('',#6068,0.225);
#2337=CIRCLE('',#6070,0.225);
#2338=CIRCLE('',#6072,1.49);
#2339=CIRCLE('',#6073,1.49);
#2340=CIRCLE('',#6075,0.71);
#2341=CIRCLE('',#6077,0.71);
#2342=CIRCLE('',#6079,2.2);
#2343=CIRCLE('',#6080,2.2);
#2344=CIRCLE('',#6086,0.976185);
#2345=CIRCLE('',#6087,0.976185);
#2346=CIRCLE('',#6088,0.247676);
#2347=CIRCLE('',#6089,0.976185);
#2348=CIRCLE('',#6090,0.976185);
#2349=CIRCLE('',#6092,0.976185);
#2350=CIRCLE('',#6094,0.5);
#2351=CIRCLE('',#6095,0.5);
#2352=CIRCLE('',#6097,0.56);
#2353=CIRCLE('',#6100,0.976185);
#2354=CIRCLE('',#6102,0.56);
#2355=CIRCLE('',#6106,1.023815);
#2356=CIRCLE('',#6107,1.023815);
#2357=CIRCLE('',#6108,0.247676);
#2358=CIRCLE('',#6109,1.023815);
#2359=CIRCLE('',#6110,1.023815);
#2360=CIRCLE('',#6112,1.023815);
#2361=CIRCLE('',#6114,1.44);
#2362=CIRCLE('',#6115,1.023815);
#2363=CIRCLE('',#6117,1.5);
#2364=CIRCLE('',#6119,1.5);
#2365=CIRCLE('',#6121,1.44);
#2366=CIRCLE('',#6126,0.23815);
#2367=CIRCLE('',#6128,0.23815);
#2368=CIRCLE('',#6130,0.23815);
#2369=CIRCLE('',#6132,0.23815);
#2370=CIRCLE('',#6134,0.23815);
#2371=CIRCLE('',#6136,0.23815);
#2372=CIRCLE('',#6138,0.23815);
#2373=CIRCLE('',#6140,0.23815);
#2374=CIRCLE('',#6143,0.243053047864041);
#2375=CIRCLE('',#6144,0.243053047864041);
#2376=CIRCLE('',#6146,1.019052);
#2377=CIRCLE('',#6147,1.019052);
#2378=CIRCLE('',#6148,1.019052);
#2379=CIRCLE('',#6149,1.019052);
#2380=CIRCLE('',#6150,1.019052);
#2381=CIRCLE('',#6151,1.019052);
#2382=CIRCLE('',#6152,1.019052);
#2383=CIRCLE('',#6153,1.019052);
#2384=CIRCLE('',#6154,1.019052);
#2385=CIRCLE('',#6156,0.980948);
#2386=CIRCLE('',#6157,0.243053047864041);
#2387=CIRCLE('',#6159,0.243053047864041);
#2388=CIRCLE('',#6161,0.980948);
#2389=CIRCLE('',#6162,0.243053047864041);
#2390=CIRCLE('',#6164,0.243053047864041);
#2391=CIRCLE('',#6166,0.980948);
#2392=CIRCLE('',#6167,0.243053047864041);
#2393=CIRCLE('',#6169,0.243053047864041);
#2394=CIRCLE('',#6171,0.980948);
#2395=CIRCLE('',#6172,0.243053047864041);
#2396=CIRCLE('',#6174,0.243053047864041);
#2397=CIRCLE('',#6176,0.980948);
#2398=CIRCLE('',#6177,0.243053047864041);
#2399=CIRCLE('',#6179,0.243053047864041);
#2400=CIRCLE('',#6181,0.980948);
#2401=CIRCLE('',#6182,0.243053047864041);
#2402=CIRCLE('',#6184,0.243053047864041);
#2403=CIRCLE('',#6186,0.980948);
#2404=CIRCLE('',#6187,0.980948);
#2405=CIRCLE('',#6188,0.980948);
#2406=CIRCLE('',#6190,0.243053047864041);
#2407=CIRCLE('',#6192,0.243053047864041);
#2408=CIRCLE('',#6197,1.013815);
#2409=CIRCLE('',#6198,0.991185);
#2410=CIRCLE('',#6200,1.013815);
#2411=CIRCLE('',#6202,0.991185);
#2412=CIRCLE('',#6205,1.013815);
#2413=CIRCLE('',#6206,0.991185);
#2414=CIRCLE('',#6208,1.013815);
#2415=CIRCLE('',#6210,0.991185);
#2416=CIRCLE('',#6219,0.6);
#2417=CIRCLE('',#6221,0.6);
#2418=CIRCLE('',#6222,0.5);
#2419=CIRCLE('',#6229,0.165);
#2420=CIRCLE('',#6231,0.165);
#2421=CIRCLE('',#6232,0.165);
#2422=CIRCLE('',#6235,0.4);
#2423=CIRCLE('',#6236,0.4);
#2424=CIRCLE('',#6238,0.225);
#2425=CIRCLE('',#6240,0.4);
#2426=CIRCLE('',#6241,0.4);
#2427=CIRCLE('',#6243,0.225);
#2428=CIRCLE('',#6246,0.225);
#2429=CIRCLE('',#6248,0.225);
#2430=CIRCLE('',#6250,0.6);
#2431=CIRCLE('',#6251,0.6);
#2432=CIRCLE('',#6264,0.17);
#2433=CIRCLE('',#6266,0.1954);
#2434=CIRCLE('',#6268,0.1954);
#2435=CIRCLE('',#6270,0.125);
#2436=CIRCLE('',#6275,0.25);
#2437=CIRCLE('',#6276,0.25);
#2438=CIRCLE('',#6278,0.25);
#2439=CIRCLE('',#6279,0.25);
#2440=CIRCLE('',#6281,0.225);
#2441=CIRCLE('',#6282,0.225);
#2442=CIRCLE('',#6284,0.8);
#2443=CIRCLE('',#6285,0.8);
#2444=CIRCLE('',#6288,1.);
#2445=CIRCLE('',#6289,0.8);
#2446=CIRCLE('',#6290,1.);
#2447=CIRCLE('',#6291,0.8);
#2448=CIRCLE('',#6292,1.);
#2449=CIRCLE('',#6295,1.);
#2450=CIRCLE('',#6297,1.);
#2451=CIRCLE('',#6299,0.8);
#2452=CIRCLE('',#6302,0.8);
#2453=CIRCLE('',#6303,1.);
#2454=CIRCLE('',#6304,0.7);
#2455=CIRCLE('',#6311,0.7);
#2456=CIRCLE('',#6312,0.5);
#2457=CIRCLE('',#6315,0.5);
#2458=CIRCLE('',#6319,0.165);
#2459=CIRCLE('',#6320,0.165);
#2460=CIRCLE('',#6323,0.6);
#2461=CIRCLE('',#6324,0.6);
#2462=CIRCLE('',#6329,0.505);
#2463=CIRCLE('',#6330,0.505);
#2464=CIRCLE('',#6332,0.7);
#2465=CIRCLE('',#6333,0.7);
#2466=CIRCLE('',#6338,0.165);
#2467=CIRCLE('',#6340,0.165);
#2468=CIRCLE('',#6343,0.505);
#2469=CIRCLE('',#6344,0.505);
#2470=CIRCLE('',#6346,0.9);
#2471=CIRCLE('',#6347,0.9);
#2472=CIRCLE('',#6352,0.3);
#2473=CIRCLE('',#6354,0.35);
#2474=CIRCLE('',#6356,0.35);
#2475=CIRCLE('',#6358,0.32);
#2476=CIRCLE('',#6360,0.22);
#2477=CIRCLE('',#6362,0.1954);
#2478=CIRCLE('',#6364,0.1954);
#2479=CIRCLE('',#6366,0.16);
#2480=CIRCLE('',#6378,0.1954);
#2481=CIRCLE('',#6387,0.17);
#2482=CIRCLE('',#6389,0.1954);
#2483=CIRCLE('',#6393,0.165);
#2484=CIRCLE('',#6394,0.165);
#2485=CIRCLE('',#6397,0.7);
#2486=CIRCLE('',#6398,0.3);
#2487=CIRCLE('',#6400,0.7);
#2488=CIRCLE('',#6401,0.3);
#2489=CIRCLE('',#6404,0.3);
#2490=CIRCLE('',#6406,0.3);
#2491=CIRCLE('',#6411,0.305);
#2492=CIRCLE('',#6412,0.305);
#2493=CIRCLE('',#6414,0.5);
#2494=CIRCLE('',#6415,0.5);
#2495=CIRCLE('',#6421,0.5);
#2496=CIRCLE('',#6422,0.5);
#2497=CIRCLE('',#6424,0.5);
#2498=CIRCLE('',#6425,0.5);
#2499=CIRCLE('',#6427,0.800000000000001);
#2500=CIRCLE('',#6428,0.800000000000001);
#2501=CIRCLE('',#6431,0.8);
#2502=CIRCLE('',#6434,0.8);
#2503=CIRCLE('',#6438,0.305);
#2504=CIRCLE('',#6439,0.305);
#2505=CIRCLE('',#6441,0.5);
#2506=CIRCLE('',#6442,0.5);
#2507=CIRCLE('',#6451,0.165);
#2508=CIRCLE('',#6452,0.165);
#2509=CIRCLE('',#6455,0.699999999999999);
#2510=CIRCLE('',#6456,0.3);
#2511=CIRCLE('',#6458,0.699999999999999);
#2512=CIRCLE('',#6459,0.3);
#2513=CIRCLE('',#6462,0.3);
#2514=CIRCLE('',#6464,0.3);
#2515=CIRCLE('',#6469,0.305);
#2516=CIRCLE('',#6470,0.305);
#2517=CIRCLE('',#6472,0.5);
#2518=CIRCLE('',#6473,0.5);
#2519=CIRCLE('',#6478,0.25);
#2520=CIRCLE('',#6479,0.25);
#2521=CIRCLE('',#6482,0.165);
#2522=CIRCLE('',#6483,0.165);
#2523=CIRCLE('',#6485,0.165);
#2524=CIRCLE('',#6486,0.165);
#2525=CIRCLE('',#6488,0.165);
#2526=CIRCLE('',#6489,0.165);
#2527=CIRCLE('',#6491,0.165);
#2528=CIRCLE('',#6492,0.165);
#2529=CIRCLE('',#6494,1.05);
#2530=CIRCLE('',#6495,1.05);
#2531=CIRCLE('',#6505,0.9);
#2532=CIRCLE('',#6508,0.9);
#2533=CIRCLE('',#6512,1.05);
#2534=CIRCLE('',#6513,0.9);
#2535=CIRCLE('',#6515,1.05);
#2536=CIRCLE('',#6517,1.);
#2537=CIRCLE('',#6519,1.);
#2538=CIRCLE('',#6521,1.05);
#2539=CIRCLE('',#6523,1.05);
#2540=CIRCLE('',#6525,1.);
#2541=CIRCLE('',#6527,1.);
#2542=CIRCLE('',#6529,1.05);
#2543=CIRCLE('',#6531,1.05);
#2544=CIRCLE('',#6533,0.9);
#2545=CIRCLE('',#6537,0.895);
#2546=CIRCLE('',#6538,0.605);
#2547=CIRCLE('',#6541,0.895);
#2548=CIRCLE('',#6542,0.605);
#2549=CIRCLE('',#6545,0.895);
#2550=CIRCLE('',#6546,0.605);
#2551=CIRCLE('',#6548,0.895);
#2552=CIRCLE('',#6550,0.605);
#2553=CIRCLE('',#6556,0.225);
#2554=CIRCLE('',#6557,0.225);
#2555=CIRCLE('',#6559,0.225);
#2556=CIRCLE('',#6560,0.225);
#2557=CIRCLE('',#6562,0.225);
#2558=CIRCLE('',#6563,0.225);
#2559=CIRCLE('',#6565,0.225);
#2560=CIRCLE('',#6566,0.225);
#2561=CIRCLE('',#6568,0.7);
#2562=CIRCLE('',#6569,0.7);
#2563=CIRCLE('',#6578,0.305);
#2564=CIRCLE('',#6579,0.305);
#2565=CIRCLE('',#6581,0.5);
#2566=CIRCLE('',#6582,0.5);
#2567=CIRCLE('',#6587,0.225);
#2568=CIRCLE('',#6588,0.225);
#2569=CIRCLE('',#6590,0.5);
#2570=CIRCLE('',#6591,0.5);
#2571=CIRCLE('',#6604,0.1954);
#2572=CIRCLE('',#6606,0.3);
#2573=CIRCLE('',#6608,0.35);
#2574=CIRCLE('',#6610,0.35);
#2575=CIRCLE('',#6612,0.32);
#2576=CIRCLE('',#6614,0.22);
#2577=CIRCLE('',#6616,0.1954);
#2578=VERTEX_POINT('',#8516);
#2579=VERTEX_POINT('',#8518);
#2580=VERTEX_POINT('',#8522);
#2581=VERTEX_POINT('',#8524);
#2582=VERTEX_POINT('',#8528);
#2583=VERTEX_POINT('',#8530);
#2584=VERTEX_POINT('',#8534);
#2585=VERTEX_POINT('',#8536);
#2586=VERTEX_POINT('',#8540);
#2587=VERTEX_POINT('',#8542);
#2588=VERTEX_POINT('',#8546);
#2589=VERTEX_POINT('',#8548);
#2590=VERTEX_POINT('',#8552);
#2591=VERTEX_POINT('',#8554);
#2592=VERTEX_POINT('',#8558);
#2593=VERTEX_POINT('',#8560);
#2594=VERTEX_POINT('',#8564);
#2595=VERTEX_POINT('',#8565);
#2596=VERTEX_POINT('',#8567);
#2597=VERTEX_POINT('',#8569);
#2598=VERTEX_POINT('',#8573);
#2599=VERTEX_POINT('',#8575);
#2600=VERTEX_POINT('',#8579);
#2601=VERTEX_POINT('',#8581);
#2602=VERTEX_POINT('',#8591);
#2603=VERTEX_POINT('',#8592);
#2604=VERTEX_POINT('',#8594);
#2605=VERTEX_POINT('',#8596);
#2606=VERTEX_POINT('',#8600);
#2607=VERTEX_POINT('',#8602);
#2608=VERTEX_POINT('',#8606);
#2609=VERTEX_POINT('',#8608);
#2610=VERTEX_POINT('',#8612);
#2611=VERTEX_POINT('',#8614);
#2612=VERTEX_POINT('',#8618);
#2613=VERTEX_POINT('',#8620);
#2614=VERTEX_POINT('',#8629);
#2615=VERTEX_POINT('',#8632);
#2616=VERTEX_POINT('',#8635);
#2617=VERTEX_POINT('',#8639);
#2618=VERTEX_POINT('',#8643);
#2619=VERTEX_POINT('',#8647);
#2620=VERTEX_POINT('',#8650);
#2621=VERTEX_POINT('',#8657);
#2622=VERTEX_POINT('',#8658);
#2623=VERTEX_POINT('',#8695);
#2624=VERTEX_POINT('',#8697);
#2625=VERTEX_POINT('',#8735);
#2626=VERTEX_POINT('',#8737);
#2627=VERTEX_POINT('',#8742);
#2628=VERTEX_POINT('',#8744);
#2629=VERTEX_POINT('',#8749);
#2630=VERTEX_POINT('',#8751);
#2631=VERTEX_POINT('',#8756);
#2632=VERTEX_POINT('',#8758);
#2633=VERTEX_POINT('',#8763);
#2634=VERTEX_POINT('',#8764);
#2635=VERTEX_POINT('',#8768);
#2636=VERTEX_POINT('',#8770);
#2637=VERTEX_POINT('',#8774);
#2638=VERTEX_POINT('',#8775);
#2639=VERTEX_POINT('',#8777);
#2640=VERTEX_POINT('',#8779);
#2641=VERTEX_POINT('',#8785);
#2642=VERTEX_POINT('',#8786);
#2643=VERTEX_POINT('',#8788);
#2644=VERTEX_POINT('',#8790);
#2645=VERTEX_POINT('',#8796);
#2646=VERTEX_POINT('',#8797);
#2647=VERTEX_POINT('',#8799);
#2648=VERTEX_POINT('',#8801);
#2649=VERTEX_POINT('',#8807);
#2650=VERTEX_POINT('',#8809);
#2651=VERTEX_POINT('',#8817);
#2652=VERTEX_POINT('',#8819);
#2653=VERTEX_POINT('',#8821);
#2654=VERTEX_POINT('',#8823);
#2655=VERTEX_POINT('',#8825);
#2656=VERTEX_POINT('',#8828);
#2657=VERTEX_POINT('',#8832);
#2658=VERTEX_POINT('',#8836);
#2659=VERTEX_POINT('',#8840);
#2660=VERTEX_POINT('',#8844);
#2661=VERTEX_POINT('',#8846);
#2662=VERTEX_POINT('',#8850);
#2663=VERTEX_POINT('',#8853);
#2664=VERTEX_POINT('',#8857);
#2665=VERTEX_POINT('',#8864);
#2666=VERTEX_POINT('',#8866);
#2667=VERTEX_POINT('',#8870);
#2668=VERTEX_POINT('',#8873);
#2669=VERTEX_POINT('',#8875);
#2670=VERTEX_POINT('',#8879);
#2671=VERTEX_POINT('',#8882);
#2672=VERTEX_POINT('',#8884);
#2673=VERTEX_POINT('',#8888);
#2674=VERTEX_POINT('',#8891);
#2675=VERTEX_POINT('',#8893);
#2676=VERTEX_POINT('',#8897);
#2677=VERTEX_POINT('',#8900);
#2678=VERTEX_POINT('',#8904);
#2679=VERTEX_POINT('',#8908);
#2680=VERTEX_POINT('',#8912);
#2681=VERTEX_POINT('',#8916);
#2682=VERTEX_POINT('',#8918);
#2683=VERTEX_POINT('',#8922);
#2684=VERTEX_POINT('',#8925);
#2685=VERTEX_POINT('',#8929);
#2686=VERTEX_POINT('',#8931);
#2687=VERTEX_POINT('',#8939);
#2688=VERTEX_POINT('',#8940);
#2689=VERTEX_POINT('',#8943);
#2690=VERTEX_POINT('',#8945);
#2691=VERTEX_POINT('',#8949);
#2692=VERTEX_POINT('',#8953);
#2693=VERTEX_POINT('',#8955);
#2694=VERTEX_POINT('',#8959);
#2695=VERTEX_POINT('',#8964);
#2696=VERTEX_POINT('',#8968);
#2697=VERTEX_POINT('',#8974);
#2698=VERTEX_POINT('',#8975);
#2699=VERTEX_POINT('',#8978);
#2700=VERTEX_POINT('',#8980);
#2701=VERTEX_POINT('',#8984);
#2702=VERTEX_POINT('',#8988);
#2703=VERTEX_POINT('',#8990);
#2704=VERTEX_POINT('',#8993);
#2705=VERTEX_POINT('',#8997);
#2706=VERTEX_POINT('',#9001);
#2707=VERTEX_POINT('',#9009);
#2708=VERTEX_POINT('',#9010);
#2709=VERTEX_POINT('',#9013);
#2710=VERTEX_POINT('',#9014);
#2711=VERTEX_POINT('',#9017);
#2712=VERTEX_POINT('',#9018);
#2713=VERTEX_POINT('',#9021);
#2714=VERTEX_POINT('',#9022);
#2715=VERTEX_POINT('',#9025);
#2716=VERTEX_POINT('',#9026);
#2717=VERTEX_POINT('',#9029);
#2718=VERTEX_POINT('',#9030);
#2719=VERTEX_POINT('',#9033);
#2720=VERTEX_POINT('',#9034);
#2721=VERTEX_POINT('',#9037);
#2722=VERTEX_POINT('',#9038);
#2723=VERTEX_POINT('',#9042);
#2724=VERTEX_POINT('',#9043);
#2725=VERTEX_POINT('',#9066);
#2726=VERTEX_POINT('',#9068);
#2727=VERTEX_POINT('',#9093);
#2728=VERTEX_POINT('',#9095);
#2729=VERTEX_POINT('',#9118);
#2730=VERTEX_POINT('',#9120);
#2731=VERTEX_POINT('',#9143);
#2732=VERTEX_POINT('',#9145);
#2733=VERTEX_POINT('',#9158);
#2734=VERTEX_POINT('',#9161);
#2735=VERTEX_POINT('',#9174);
#2736=VERTEX_POINT('',#9176);
#2737=VERTEX_POINT('',#9199);
#2738=VERTEX_POINT('',#9201);
#2739=VERTEX_POINT('',#9224);
#2740=VERTEX_POINT('',#9226);
#2741=VERTEX_POINT('',#9249);
#2742=VERTEX_POINT('',#9251);
#2743=VERTEX_POINT('',#9276);
#2744=VERTEX_POINT('',#9280);
#2745=VERTEX_POINT('',#9305);
#2746=VERTEX_POINT('',#9309);
#2747=VERTEX_POINT('',#9334);
#2748=VERTEX_POINT('',#9338);
#2749=VERTEX_POINT('',#9339);
#2750=VERTEX_POINT('',#9366);
#2751=VERTEX_POINT('',#9370);
#2752=VERTEX_POINT('',#9395);
#2753=VERTEX_POINT('',#9399);
#2754=VERTEX_POINT('',#9424);
#2755=VERTEX_POINT('',#9428);
#2756=VERTEX_POINT('',#9453);
#2757=VERTEX_POINT('',#9456);
#2758=VERTEX_POINT('',#9458);
#2759=VERTEX_POINT('',#9490);
#2760=VERTEX_POINT('',#9492);
#2761=VERTEX_POINT('',#9495);
#2762=VERTEX_POINT('',#9499);
#2763=VERTEX_POINT('',#9504);
#2764=VERTEX_POINT('',#9506);
#2765=VERTEX_POINT('',#9509);
#2766=VERTEX_POINT('',#9513);
#2767=VERTEX_POINT('',#9524);
#2768=VERTEX_POINT('',#9527);
#2769=VERTEX_POINT('',#9529);
#2770=VERTEX_POINT('',#9537);
#2771=VERTEX_POINT('',#9538);
#2772=VERTEX_POINT('',#9540);
#2773=VERTEX_POINT('',#9542);
#2774=VERTEX_POINT('',#9546);
#2775=VERTEX_POINT('',#9547);
#2776=VERTEX_POINT('',#9549);
#2777=VERTEX_POINT('',#9551);
#2778=VERTEX_POINT('',#9555);
#2779=VERTEX_POINT('',#9556);
#2780=VERTEX_POINT('',#9560);
#2781=VERTEX_POINT('',#9561);
#2782=VERTEX_POINT('',#9568);
#2783=VERTEX_POINT('',#9570);
#2784=VERTEX_POINT('',#9589);
#2785=VERTEX_POINT('',#9595);
#2786=VERTEX_POINT('',#9597);
#2787=VERTEX_POINT('',#9601);
#2788=VERTEX_POINT('',#9604);
#2789=VERTEX_POINT('',#9606);
#2790=VERTEX_POINT('',#9610);
#2791=VERTEX_POINT('',#9616);
#2792=VERTEX_POINT('',#9620);
#2793=VERTEX_POINT('',#9624);
#2794=VERTEX_POINT('',#9627);
#2795=VERTEX_POINT('',#9637);
#2796=VERTEX_POINT('',#9638);
#2797=VERTEX_POINT('',#9640);
#2798=VERTEX_POINT('',#9642);
#2799=VERTEX_POINT('',#9646);
#2800=VERTEX_POINT('',#9648);
#2801=VERTEX_POINT('',#9652);
#2802=VERTEX_POINT('',#9654);
#2803=VERTEX_POINT('',#9658);
#2804=VERTEX_POINT('',#9660);
#2805=VERTEX_POINT('',#9664);
#2806=VERTEX_POINT('',#9666);
#2807=VERTEX_POINT('',#9674);
#2808=VERTEX_POINT('',#9677);
#2809=VERTEX_POINT('',#9681);
#2810=VERTEX_POINT('',#9685);
#2811=VERTEX_POINT('',#9692);
#2812=VERTEX_POINT('',#9694);
#2813=VERTEX_POINT('',#9698);
#2814=VERTEX_POINT('',#9700);
#2815=VERTEX_POINT('',#9704);
#2816=VERTEX_POINT('',#9706);
#2817=VERTEX_POINT('',#9710);
#2818=VERTEX_POINT('',#9711);
#2819=VERTEX_POINT('',#9713);
#2820=VERTEX_POINT('',#9715);
#2821=VERTEX_POINT('',#9719);
#2822=VERTEX_POINT('',#9721);
#2823=VERTEX_POINT('',#9725);
#2824=VERTEX_POINT('',#9727);
#2825=VERTEX_POINT('',#9729);
#2826=VERTEX_POINT('',#9731);
#2827=VERTEX_POINT('',#9733);
#2828=VERTEX_POINT('',#9735);
#2829=VERTEX_POINT('',#9737);
#2830=VERTEX_POINT('',#9739);
#2831=VERTEX_POINT('',#9741);
#2832=VERTEX_POINT('',#9745);
#2833=VERTEX_POINT('',#9749);
#2834=VERTEX_POINT('',#9753);
#2835=VERTEX_POINT('',#9757);
#2836=VERTEX_POINT('',#9759);
#2837=VERTEX_POINT('',#9763);
#2838=VERTEX_POINT('',#9767);
#2839=VERTEX_POINT('',#9769);
#2840=VERTEX_POINT('',#9771);
#2841=VERTEX_POINT('',#9775);
#2842=VERTEX_POINT('',#9786);
#2843=VERTEX_POINT('',#9788);
#2844=VERTEX_POINT('',#9793);
#2845=VERTEX_POINT('',#9799);
#2846=VERTEX_POINT('',#9801);
#2847=VERTEX_POINT('',#9806);
#2848=VERTEX_POINT('',#9808);
#2849=VERTEX_POINT('',#9815);
#2850=VERTEX_POINT('',#9817);
#2851=VERTEX_POINT('',#9821);
#2852=VERTEX_POINT('',#9823);
#2853=VERTEX_POINT('',#9830);
#2854=VERTEX_POINT('',#9831);
#2855=VERTEX_POINT('',#9835);
#2856=VERTEX_POINT('',#9850);
#2857=VERTEX_POINT('',#9852);
#2858=VERTEX_POINT('',#9861);
#2859=VERTEX_POINT('',#9863);
#2860=VERTEX_POINT('',#9911);
#2861=VERTEX_POINT('',#9913);
#2862=VERTEX_POINT('',#9917);
#2863=VERTEX_POINT('',#9919);
#2864=VERTEX_POINT('',#9926);
#2865=VERTEX_POINT('',#9929);
#2866=VERTEX_POINT('',#9933);
#2867=VERTEX_POINT('',#9937);
#2868=VERTEX_POINT('',#9941);
#2869=VERTEX_POINT('',#9944);
#2870=VERTEX_POINT('',#9948);
#2871=VERTEX_POINT('',#9952);
#2872=VERTEX_POINT('',#9957);
#2873=VERTEX_POINT('',#9958);
#2874=VERTEX_POINT('',#9960);
#2875=VERTEX_POINT('',#9962);
#2876=VERTEX_POINT('',#9966);
#2877=VERTEX_POINT('',#9968);
#2878=VERTEX_POINT('',#9972);
#2879=VERTEX_POINT('',#9974);
#2880=VERTEX_POINT('',#9978);
#2881=VERTEX_POINT('',#9980);
#2882=VERTEX_POINT('',#9984);
#2883=VERTEX_POINT('',#9986);
#2884=VERTEX_POINT('',#9996);
#2885=VERTEX_POINT('',#9999);
#2886=VERTEX_POINT('',#10000);
#2887=VERTEX_POINT('',#10002);
#2888=VERTEX_POINT('',#10004);
#2889=VERTEX_POINT('',#10008);
#2890=VERTEX_POINT('',#10010);
#2891=VERTEX_POINT('',#10014);
#2892=VERTEX_POINT('',#10016);
#2893=VERTEX_POINT('',#10020);
#2894=VERTEX_POINT('',#10022);
#2895=VERTEX_POINT('',#10026);
#2896=VERTEX_POINT('',#10028);
#2897=VERTEX_POINT('',#10036);
#2898=VERTEX_POINT('',#10039);
#2899=VERTEX_POINT('',#10046);
#2900=VERTEX_POINT('',#10048);
#2901=VERTEX_POINT('',#10053);
#2902=VERTEX_POINT('',#10055);
#2903=VERTEX_POINT('',#10058);
#2904=VERTEX_POINT('',#10060);
#2905=VERTEX_POINT('',#10065);
#2906=VERTEX_POINT('',#10069);
#2907=VERTEX_POINT('',#10076);
#2908=VERTEX_POINT('',#10078);
#2909=VERTEX_POINT('',#10082);
#2910=VERTEX_POINT('',#10084);
#2911=VERTEX_POINT('',#10092);
#2912=VERTEX_POINT('',#10094);
#2913=VERTEX_POINT('',#10098);
#2914=VERTEX_POINT('',#10100);
#2915=VERTEX_POINT('',#10104);
#2916=VERTEX_POINT('',#10105);
#2917=VERTEX_POINT('',#10107);
#2918=VERTEX_POINT('',#10109);
#2919=VERTEX_POINT('',#10113);
#2920=VERTEX_POINT('',#10115);
#2921=VERTEX_POINT('',#10119);
#2922=VERTEX_POINT('',#10123);
#2923=VERTEX_POINT('',#10131);
#2924=VERTEX_POINT('',#10133);
#2925=VERTEX_POINT('',#10137);
#2926=VERTEX_POINT('',#10139);
#2927=VERTEX_POINT('',#10150);
#2928=VERTEX_POINT('',#10152);
#2929=VERTEX_POINT('',#10157);
#2930=VERTEX_POINT('',#10159);
#2931=VERTEX_POINT('',#10162);
#2932=VERTEX_POINT('',#10164);
#2933=VERTEX_POINT('',#10169);
#2934=VERTEX_POINT('',#10173);
#2935=VERTEX_POINT('',#10180);
#2936=VERTEX_POINT('',#10182);
#2937=VERTEX_POINT('',#10186);
#2938=VERTEX_POINT('',#10188);
#2939=VERTEX_POINT('',#10195);
#2940=VERTEX_POINT('',#10197);
#2941=VERTEX_POINT('',#10202);
#2942=VERTEX_POINT('',#10204);
#2943=VERTEX_POINT('',#10208);
#2944=VERTEX_POINT('',#10210);
#2945=VERTEX_POINT('',#10214);
#2946=VERTEX_POINT('',#10216);
#2947=VERTEX_POINT('',#10220);
#2948=VERTEX_POINT('',#10222);
#2949=VERTEX_POINT('',#10226);
#2950=VERTEX_POINT('',#10228);
#2951=VERTEX_POINT('',#10232);
#2952=VERTEX_POINT('',#10233);
#2953=VERTEX_POINT('',#10235);
#2954=VERTEX_POINT('',#10237);
#2955=VERTEX_POINT('',#10241);
#2956=VERTEX_POINT('',#10243);
#2957=VERTEX_POINT('',#10247);
#2958=VERTEX_POINT('',#10249);
#2959=VERTEX_POINT('',#10260);
#2960=VERTEX_POINT('',#10261);
#2961=VERTEX_POINT('',#10263);
#2962=VERTEX_POINT('',#10265);
#2963=VERTEX_POINT('',#10269);
#2964=VERTEX_POINT('',#10271);
#2965=VERTEX_POINT('',#10275);
#2966=VERTEX_POINT('',#10277);
#2967=VERTEX_POINT('',#10285);
#2968=VERTEX_POINT('',#10287);
#2969=VERTEX_POINT('',#10290);
#2970=VERTEX_POINT('',#10294);
#2971=VERTEX_POINT('',#10297);
#2972=VERTEX_POINT('',#10301);
#2973=VERTEX_POINT('',#10304);
#2974=VERTEX_POINT('',#10308);
#2975=VERTEX_POINT('',#10311);
#2976=VERTEX_POINT('',#10315);
#2977=VERTEX_POINT('',#10318);
#2978=VERTEX_POINT('',#10322);
#2979=VERTEX_POINT('',#10328);
#2980=VERTEX_POINT('',#10329);
#2981=VERTEX_POINT('',#10331);
#2982=VERTEX_POINT('',#10333);
#2983=VERTEX_POINT('',#10337);
#2984=VERTEX_POINT('',#10339);
#2985=VERTEX_POINT('',#10343);
#2986=VERTEX_POINT('',#10345);
#2987=VERTEX_POINT('',#10352);
#2988=VERTEX_POINT('',#10354);
#2989=VERTEX_POINT('',#10357);
#2990=VERTEX_POINT('',#10361);
#2991=VERTEX_POINT('',#10369);
#2992=VERTEX_POINT('',#10371);
#2993=VERTEX_POINT('',#10375);
#2994=VERTEX_POINT('',#10377);
#2995=VERTEX_POINT('',#10381);
#2996=VERTEX_POINT('',#10383);
#2997=VERTEX_POINT('',#10387);
#2998=VERTEX_POINT('',#10389);
#2999=VERTEX_POINT('',#10393);
#3000=VERTEX_POINT('',#10395);
#3001=VERTEX_POINT('',#10399);
#3002=VERTEX_POINT('',#10400);
#3003=VERTEX_POINT('',#10402);
#3004=VERTEX_POINT('',#10404);
#3005=VERTEX_POINT('',#10408);
#3006=VERTEX_POINT('',#10410);
#3007=VERTEX_POINT('',#10414);
#3008=VERTEX_POINT('',#10416);
#3009=VERTEX_POINT('',#10426);
#3010=VERTEX_POINT('',#10428);
#3011=VERTEX_POINT('',#10432);
#3012=VERTEX_POINT('',#10434);
#3013=VERTEX_POINT('',#10441);
#3014=VERTEX_POINT('',#10443);
#3015=VERTEX_POINT('',#10447);
#3016=VERTEX_POINT('',#10449);
#3017=VERTEX_POINT('',#10456);
#3018=VERTEX_POINT('',#10457);
#3019=VERTEX_POINT('',#10459);
#3020=VERTEX_POINT('',#10461);
#3021=VERTEX_POINT('',#10465);
#3022=VERTEX_POINT('',#10467);
#3023=VERTEX_POINT('',#10471);
#3024=VERTEX_POINT('',#10473);
#3025=VERTEX_POINT('',#10477);
#3026=VERTEX_POINT('',#10479);
#3027=VERTEX_POINT('',#10483);
#3028=VERTEX_POINT('',#10485);
#3029=VERTEX_POINT('',#10494);
#3030=VERTEX_POINT('',#10497);
#3031=VERTEX_POINT('',#10500);
#3032=VERTEX_POINT('',#10504);
#3033=VERTEX_POINT('',#10508);
#3034=VERTEX_POINT('',#10512);
#3035=VERTEX_POINT('',#10515);
#3036=EDGE_CURVE('',#2578,#2578,#2259,.T.);
#3037=EDGE_CURVE('',#2578,#2579,#1601,.T.);
#3038=EDGE_CURVE('',#2579,#2579,#2260,.T.);
#3039=EDGE_CURVE('',#2580,#2580,#2261,.T.);
#3040=EDGE_CURVE('',#2580,#2581,#1602,.T.);
#3041=EDGE_CURVE('',#2581,#2581,#2262,.T.);
#3042=EDGE_CURVE('',#2582,#2582,#2263,.T.);
#3043=EDGE_CURVE('',#2582,#2583,#1603,.T.);
#3044=EDGE_CURVE('',#2583,#2583,#2264,.T.);
#3045=EDGE_CURVE('',#2584,#2584,#2265,.T.);
#3046=EDGE_CURVE('',#2584,#2585,#1604,.T.);
#3047=EDGE_CURVE('',#2585,#2585,#2266,.T.);
#3048=EDGE_CURVE('',#2586,#2586,#2267,.T.);
#3049=EDGE_CURVE('',#2586,#2587,#1605,.T.);
#3050=EDGE_CURVE('',#2587,#2587,#2268,.T.);
#3051=EDGE_CURVE('',#2588,#2588,#2269,.T.);
#3052=EDGE_CURVE('',#2588,#2589,#1606,.T.);
#3053=EDGE_CURVE('',#2589,#2589,#2270,.T.);
#3054=EDGE_CURVE('',#2590,#2590,#2271,.T.);
#3055=EDGE_CURVE('',#2590,#2591,#1607,.T.);
#3056=EDGE_CURVE('',#2591,#2591,#2272,.T.);
#3057=EDGE_CURVE('',#2592,#2592,#2273,.T.);
#3058=EDGE_CURVE('',#2592,#2593,#1608,.T.);
#3059=EDGE_CURVE('',#2593,#2593,#2274,.T.);
#3060=EDGE_CURVE('',#2594,#2595,#1609,.T.);
#3061=EDGE_CURVE('',#2595,#2596,#1610,.T.);
#3062=EDGE_CURVE('',#2597,#2596,#1611,.T.);
#3063=EDGE_CURVE('',#2594,#2597,#1612,.T.);
#3064=EDGE_CURVE('',#2598,#2594,#1613,.T.);
#3065=EDGE_CURVE('',#2599,#2597,#1614,.T.);
#3066=EDGE_CURVE('',#2598,#2599,#1615,.T.);
#3067=EDGE_CURVE('',#2600,#2598,#1616,.T.);
#3068=EDGE_CURVE('',#2601,#2599,#1617,.T.);
#3069=EDGE_CURVE('',#2600,#2601,#1618,.T.);
#3070=EDGE_CURVE('',#2595,#2600,#1619,.T.);
#3071=EDGE_CURVE('',#2596,#2601,#1620,.T.);
#3072=EDGE_CURVE('',#2602,#2603,#1621,.T.);
#3073=EDGE_CURVE('',#2603,#2604,#1622,.T.);
#3074=EDGE_CURVE('',#2604,#2605,#1623,.T.);
#3075=EDGE_CURVE('',#2602,#2605,#1624,.T.);
#3076=EDGE_CURVE('',#2603,#2606,#1625,.T.);
#3077=EDGE_CURVE('',#2606,#2607,#1626,.T.);
#3078=EDGE_CURVE('',#2607,#2604,#1627,.T.);
#3079=EDGE_CURVE('',#2606,#2608,#1628,.T.);
#3080=EDGE_CURVE('',#2608,#2609,#1629,.T.);
#3081=EDGE_CURVE('',#2609,#2607,#1630,.T.);
#3082=EDGE_CURVE('',#2608,#2610,#1631,.T.);
#3083=EDGE_CURVE('',#2610,#2611,#1632,.T.);
#3084=EDGE_CURVE('',#2611,#2609,#1633,.T.);
#3085=EDGE_CURVE('',#2610,#2612,#1634,.T.);
#3086=EDGE_CURVE('',#2612,#2613,#1635,.T.);
#3087=EDGE_CURVE('',#2613,#2611,#1636,.T.);
#3088=EDGE_CURVE('',#2612,#2602,#1637,.T.);
#3089=EDGE_CURVE('',#2605,#2613,#1638,.T.);
#3090=EDGE_CURVE('',#2614,#2614,#2275,.T.);
#3091=EDGE_CURVE('',#2615,#2615,#2276,.T.);
#3092=EDGE_CURVE('',#2616,#2616,#2277,.T.);
#3093=EDGE_CURVE('',#2616,#2615,#1639,.T.);
#3094=EDGE_CURVE('',#2617,#2617,#2278,.T.);
#3095=EDGE_CURVE('',#2617,#2616,#1640,.T.);
#3096=EDGE_CURVE('',#2618,#2618,#2279,.T.);
#3097=EDGE_CURVE('',#2618,#2617,#1641,.T.);
#3098=EDGE_CURVE('',#2619,#2619,#2280,.T.);
#3099=EDGE_CURVE('',#2620,#2620,#2281,.F.);
#3100=EDGE_CURVE('',#2620,#2619,#1642,.T.);
#3101=EDGE_CURVE('',#2614,#2620,#1643,.T.);
#3102=EDGE_CURVE('',#2621,#2622,#281,.T.);
#3103=EDGE_CURVE('',#2622,#2621,#282,.T.);
#3104=EDGE_CURVE('',#2622,#2623,#1644,.T.);
#3105=EDGE_CURVE('',#2624,#2623,#283,.T.);
#3106=EDGE_CURVE('',#2623,#2624,#284,.T.);
#3107=EDGE_CURVE('',#2625,#2625,#2282,.T.);
#3108=EDGE_CURVE('',#2625,#2626,#1645,.T.);
#3109=EDGE_CURVE('',#2626,#2626,#2283,.T.);
#3110=EDGE_CURVE('',#2627,#2627,#2284,.T.);
#3111=EDGE_CURVE('',#2627,#2628,#1646,.T.);
#3112=EDGE_CURVE('',#2628,#2628,#2285,.T.);
#3113=EDGE_CURVE('',#2629,#2629,#2286,.T.);
#3114=EDGE_CURVE('',#2629,#2630,#1647,.T.);
#3115=EDGE_CURVE('',#2630,#2630,#2287,.T.);
#3116=EDGE_CURVE('',#2631,#2631,#2288,.T.);
#3117=EDGE_CURVE('',#2631,#2632,#1648,.T.);
#3118=EDGE_CURVE('',#2632,#2632,#2289,.T.);
#3119=EDGE_CURVE('',#2633,#2634,#2290,.T.);
#3120=EDGE_CURVE('',#2634,#2633,#2291,.T.);
#3121=EDGE_CURVE('',#2635,#2633,#1649,.T.);
#3122=EDGE_CURVE('',#2636,#2635,#2292,.T.);
#3123=EDGE_CURVE('',#2634,#2636,#1650,.T.);
#3124=EDGE_CURVE('',#2637,#2638,#1651,.T.);
#3125=EDGE_CURVE('',#2637,#2639,#2293,.T.);
#3126=EDGE_CURVE('',#2640,#2639,#1652,.T.);
#3127=EDGE_CURVE('',#2638,#2640,#2294,.T.);
#3128=EDGE_CURVE('',#2639,#2637,#2295,.T.);
#3129=EDGE_CURVE('',#2641,#2642,#1653,.T.);
#3130=EDGE_CURVE('',#2641,#2643,#2296,.T.);
#3131=EDGE_CURVE('',#2644,#2643,#1654,.T.);
#3132=EDGE_CURVE('',#2642,#2644,#2297,.T.);
#3133=EDGE_CURVE('',#2643,#2641,#2298,.T.);
#3134=EDGE_CURVE('',#2645,#2646,#1655,.T.);
#3135=EDGE_CURVE('',#2645,#2647,#2299,.T.);
#3136=EDGE_CURVE('',#2648,#2647,#1656,.T.);
#3137=EDGE_CURVE('',#2646,#2648,#2300,.T.);
#3138=EDGE_CURVE('',#2647,#2645,#2301,.T.);
#3139=EDGE_CURVE('',#2649,#2649,#2302,.T.);
#3140=EDGE_CURVE('',#2649,#2650,#1657,.T.);
#3141=EDGE_CURVE('',#2650,#2635,#2303,.T.);
#3142=EDGE_CURVE('',#2636,#2648,#2304,.T.);
#3143=EDGE_CURVE('',#2646,#2644,#2305,.T.);
#3144=EDGE_CURVE('',#2642,#2640,#2306,.T.);
#3145=EDGE_CURVE('',#2638,#2650,#2307,.T.);
#3146=EDGE_CURVE('',#2651,#2651,#2308,.T.);
#3147=EDGE_CURVE('',#2652,#2652,#2309,.T.);
#3148=EDGE_CURVE('',#2653,#2653,#2310,.T.);
#3149=EDGE_CURVE('',#2654,#2654,#2311,.T.);
#3150=EDGE_CURVE('',#2655,#2655,#2312,.T.);
#3151=EDGE_CURVE('',#2656,#2656,#2313,.T.);
#3152=EDGE_CURVE('',#2656,#2652,#1658,.T.);
#3153=EDGE_CURVE('',#2657,#2657,#2314,.T.);
#3154=EDGE_CURVE('',#2657,#2655,#1659,.T.);
#3155=EDGE_CURVE('',#2658,#2658,#2315,.T.);
#3156=EDGE_CURVE('',#2658,#2653,#1660,.T.);
#3157=EDGE_CURVE('',#2659,#2659,#2316,.T.);
#3158=EDGE_CURVE('',#2659,#2654,#1661,.T.);
#3159=EDGE_CURVE('',#2660,#2660,#2317,.T.);
#3160=EDGE_CURVE('',#2660,#2661,#1662,.T.);
#3161=EDGE_CURVE('',#2661,#2661,#2318,.T.);
#3162=EDGE_CURVE('',#2662,#2662,#2319,.T.);
#3163=EDGE_CURVE('',#2651,#2663,#1663,.T.);
#3164=EDGE_CURVE('',#2663,#2663,#2320,.T.);
#3165=EDGE_CURVE('',#2662,#2664,#1664,.T.);
#3166=EDGE_CURVE('',#2664,#2664,#2321,.T.);
#3167=EDGE_CURVE('',#2665,#2665,#2322,.T.);
#3168=EDGE_CURVE('',#2665,#2666,#1665,.T.);
#3169=EDGE_CURVE('',#2666,#2666,#2323,.T.);
#3170=EDGE_CURVE('',#2667,#2667,#2324,.T.);
#3171=EDGE_CURVE('',#2668,#2668,#2325,.T.);
#3172=EDGE_CURVE('',#2668,#2669,#1666,.T.);
#3173=EDGE_CURVE('',#2669,#2669,#2326,.T.);
#3174=EDGE_CURVE('',#2670,#2670,#2327,.T.);
#3175=EDGE_CURVE('',#2671,#2671,#2328,.T.);
#3176=EDGE_CURVE('',#2671,#2672,#1667,.T.);
#3177=EDGE_CURVE('',#2672,#2672,#2329,.T.);
#3178=EDGE_CURVE('',#2673,#2673,#2330,.T.);
#3179=EDGE_CURVE('',#2674,#2674,#2331,.T.);
#3180=EDGE_CURVE('',#2674,#2675,#1668,.T.);
#3181=EDGE_CURVE('',#2675,#2675,#2332,.T.);
#3182=EDGE_CURVE('',#2676,#2676,#2333,.T.);
#3183=EDGE_CURVE('',#2677,#2677,#2334,.T.);
#3184=EDGE_CURVE('',#2677,#2667,#1669,.T.);
#3185=EDGE_CURVE('',#2678,#2678,#2335,.T.);
#3186=EDGE_CURVE('',#2678,#2670,#1670,.T.);
#3187=EDGE_CURVE('',#2679,#2679,#2336,.T.);
#3188=EDGE_CURVE('',#2679,#2673,#1671,.T.);
#3189=EDGE_CURVE('',#2680,#2680,#2337,.T.);
#3190=EDGE_CURVE('',#2680,#2676,#1672,.T.);
#3191=EDGE_CURVE('',#2681,#2681,#2338,.T.);
#3192=EDGE_CURVE('',#2681,#2682,#1673,.T.);
#3193=EDGE_CURVE('',#2682,#2682,#2339,.T.);
#3194=EDGE_CURVE('',#2683,#2683,#2340,.T.);
#3195=EDGE_CURVE('',#2684,#2684,#2341,.T.);
#3196=EDGE_CURVE('',#2684,#2683,#1674,.T.);
#3197=EDGE_CURVE('',#2685,#2685,#2342,.T.);
#3198=EDGE_CURVE('',#2685,#2686,#1675,.T.);
#3199=EDGE_CURVE('',#2686,#2686,#2343,.T.);
#3200=EDGE_CURVE('',#2687,#2688,#2344,.T.);
#3201=EDGE_CURVE('',#2688,#2687,#2345,.T.);
#3202=EDGE_CURVE('',#2688,#2689,#2346,.T.);
#3203=EDGE_CURVE('',#2690,#2689,#2347,.T.);
#3204=EDGE_CURVE('',#2689,#2690,#2348,.T.);
#3205=EDGE_CURVE('',#2690,#2691,#1676,.T.);
#3206=EDGE_CURVE('',#2691,#2691,#2349,.T.);
#3207=EDGE_CURVE('',#2692,#2692,#2350,.T.);
#3208=EDGE_CURVE('',#2692,#2693,#1677,.T.);
#3209=EDGE_CURVE('',#2693,#2693,#2351,.T.);
#3210=EDGE_CURVE('',#2693,#2694,#1678,.T.);
#3211=EDGE_CURVE('',#2694,#2694,#2352,.T.);
#3212=EDGE_CURVE('',#2695,#2695,#2353,.T.);
#3213=EDGE_CURVE('',#2695,#2687,#1679,.T.);
#3214=EDGE_CURVE('',#2696,#2696,#2354,.T.);
#3215=EDGE_CURVE('',#2696,#2692,#1680,.T.);
#3216=EDGE_CURVE('',#2697,#2698,#2355,.T.);
#3217=EDGE_CURVE('',#2698,#2697,#2356,.T.);
#3218=EDGE_CURVE('',#2698,#2699,#2357,.T.);
#3219=EDGE_CURVE('',#2700,#2699,#2358,.T.);
#3220=EDGE_CURVE('',#2699,#2700,#2359,.T.);
#3221=EDGE_CURVE('',#2701,#2701,#2360,.T.);
#3222=EDGE_CURVE('',#2701,#2700,#1681,.T.);
#3223=EDGE_CURVE('',#2702,#2702,#2361,.T.);
#3224=EDGE_CURVE('',#2703,#2703,#2362,.T.);
#3225=EDGE_CURVE('',#2704,#2704,#2363,.T.);
#3226=EDGE_CURVE('',#2704,#2702,#1682,.T.);
#3227=EDGE_CURVE('',#2705,#2705,#2364,.T.);
#3228=EDGE_CURVE('',#2705,#2704,#1683,.T.);
#3229=EDGE_CURVE('',#2706,#2706,#2365,.T.);
#3230=EDGE_CURVE('',#2706,#2705,#1684,.T.);
#3231=EDGE_CURVE('',#2697,#2703,#1685,.T.);
#3232=EDGE_CURVE('',#2707,#2708,#2366,.T.);
#3233=EDGE_CURVE('',#2709,#2710,#2367,.T.);
#3234=EDGE_CURVE('',#2711,#2712,#2368,.T.);
#3235=EDGE_CURVE('',#2713,#2714,#2369,.T.);
#3236=EDGE_CURVE('',#2715,#2716,#2370,.T.);
#3237=EDGE_CURVE('',#2717,#2718,#2371,.T.);
#3238=EDGE_CURVE('',#2719,#2720,#2372,.T.);
#3239=EDGE_CURVE('',#2721,#2722,#2373,.T.);
#3240=EDGE_CURVE('',#2723,#2724,#285,.T.);
#3241=EDGE_CURVE('',#2725,#2723,#2374,.T.);
#3242=EDGE_CURVE('',#2726,#2725,#286,.T.);
#3243=EDGE_CURVE('',#2724,#2726,#2375,.T.);
#3244=EDGE_CURVE('',#2727,#2725,#2376,.T.);
#3245=EDGE_CURVE('',#2727,#2728,#287,.T.);
#3246=EDGE_CURVE('',#2729,#2728,#2377,.T.);
#3247=EDGE_CURVE('',#2729,#2730,#288,.T.);
#3248=EDGE_CURVE('',#2731,#2730,#2378,.T.);
#3249=EDGE_CURVE('',#2731,#2732,#289,.T.);
#3250=EDGE_CURVE('',#2732,#2733,#1686,.T.);
#3251=EDGE_CURVE('',#2733,#2733,#2379,.T.);
#3252=EDGE_CURVE('',#2732,#2734,#290,.T.);
#3253=EDGE_CURVE('',#2735,#2734,#2380,.T.);
#3254=EDGE_CURVE('',#2735,#2736,#291,.T.);
#3255=EDGE_CURVE('',#2737,#2736,#2381,.T.);
#3256=EDGE_CURVE('',#2737,#2738,#292,.T.);
#3257=EDGE_CURVE('',#2739,#2738,#2382,.T.);
#3258=EDGE_CURVE('',#2739,#2740,#293,.T.);
#3259=EDGE_CURVE('',#2741,#2740,#2383,.T.);
#3260=EDGE_CURVE('',#2741,#2742,#294,.T.);
#3261=EDGE_CURVE('',#2726,#2742,#2384,.T.);
#3262=EDGE_CURVE('',#2723,#2743,#2385,.T.);
#3263=EDGE_CURVE('',#2743,#2727,#2386,.T.);
#3264=EDGE_CURVE('',#2744,#2743,#295,.T.);
#3265=EDGE_CURVE('',#2728,#2744,#2387,.T.);
#3266=EDGE_CURVE('',#2744,#2745,#2388,.T.);
#3267=EDGE_CURVE('',#2745,#2729,#2389,.T.);
#3268=EDGE_CURVE('',#2746,#2745,#296,.T.);
#3269=EDGE_CURVE('',#2730,#2746,#2390,.T.);
#3270=EDGE_CURVE('',#2746,#2747,#2391,.T.);
#3271=EDGE_CURVE('',#2747,#2731,#2392,.T.);
#3272=EDGE_CURVE('',#2748,#2749,#297,.T.);
#3273=EDGE_CURVE('',#2734,#2748,#2393,.T.);
#3274=EDGE_CURVE('',#2749,#2747,#298,.T.);
#3275=EDGE_CURVE('',#2748,#2750,#2394,.T.);
#3276=EDGE_CURVE('',#2750,#2735,#2395,.T.);
#3277=EDGE_CURVE('',#2751,#2750,#299,.T.);
#3278=EDGE_CURVE('',#2736,#2751,#2396,.T.);
#3279=EDGE_CURVE('',#2751,#2752,#2397,.T.);
#3280=EDGE_CURVE('',#2752,#2737,#2398,.T.);
#3281=EDGE_CURVE('',#2753,#2752,#300,.T.);
#3282=EDGE_CURVE('',#2738,#2753,#2399,.T.);
#3283=EDGE_CURVE('',#2753,#2754,#2400,.T.);
#3284=EDGE_CURVE('',#2754,#2739,#2401,.T.);
#3285=EDGE_CURVE('',#2755,#2754,#301,.T.);
#3286=EDGE_CURVE('',#2740,#2755,#2402,.T.);
#3287=EDGE_CURVE('',#2756,#2756,#2403,.T.);
#3288=EDGE_CURVE('',#2756,#2749,#1687,.T.);
#3289=EDGE_CURVE('',#2757,#2724,#2404,.T.);
#3290=EDGE_CURVE('',#2757,#2758,#302,.T.);
#3291=EDGE_CURVE('',#2755,#2758,#2405,.T.);
#3292=EDGE_CURVE('',#2742,#2757,#2406,.T.);
#3293=EDGE_CURVE('',#2758,#2741,#2407,.T.);
#3294=EDGE_CURVE('',#2759,#2759,#2408,.T.);
#3295=EDGE_CURVE('',#2760,#2760,#2409,.T.);
#3296=EDGE_CURVE('',#2761,#2761,#2410,.T.);
#3297=EDGE_CURVE('',#2761,#2759,#1688,.T.);
#3298=EDGE_CURVE('',#2762,#2762,#2411,.T.);
#3299=EDGE_CURVE('',#2762,#2760,#1689,.T.);
#3300=EDGE_CURVE('',#2763,#2763,#2412,.T.);
#3301=EDGE_CURVE('',#2764,#2764,#2413,.T.);
#3302=EDGE_CURVE('',#2765,#2765,#2414,.T.);
#3303=EDGE_CURVE('',#2765,#2763,#1690,.T.);
#3304=EDGE_CURVE('',#2766,#2766,#2415,.T.);
#3305=EDGE_CURVE('',#2766,#2764,#1691,.T.);
#3306=EDGE_CURVE('',#2767,#2767,#2416,.T.);
#3307=EDGE_CURVE('',#2768,#2768,#2417,.T.);
#3308=EDGE_CURVE('',#2768,#2769,#1692,.T.);
#3309=EDGE_CURVE('',#2769,#2769,#2418,.T.);
#3310=EDGE_CURVE('',#2767,#2768,#1693,.T.);
#3311=EDGE_CURVE('',#2770,#2771,#1694,.T.);
#3312=EDGE_CURVE('',#2771,#2772,#1695,.T.);
#3313=EDGE_CURVE('',#2772,#2773,#1696,.T.);
#3314=EDGE_CURVE('',#2773,#2770,#1697,.T.);
#3315=EDGE_CURVE('',#2774,#2775,#1698,.T.);
#3316=EDGE_CURVE('',#2775,#2776,#1699,.T.);
#3317=EDGE_CURVE('',#2776,#2777,#1700,.T.);
#3318=EDGE_CURVE('',#2777,#2774,#1701,.T.);
#3319=EDGE_CURVE('',#2778,#2779,#1702,.T.);
#3320=EDGE_CURVE('',#2778,#2779,#2419,.T.);
#3321=EDGE_CURVE('',#2780,#2781,#303,.T.);
#3322=EDGE_CURVE('',#2782,#2780,#2420,.T.);
#3323=EDGE_CURVE('',#2783,#2782,#304,.T.);
#3324=EDGE_CURVE('',#2779,#2783,#305,.T.);
#3325=EDGE_CURVE('',#2781,#2778,#306,.T.);
#3326=EDGE_CURVE('',#2781,#2784,#1703,.T.);
#3327=EDGE_CURVE('',#2784,#2784,#2421,.T.);
#3328=EDGE_CURVE('',#2782,#2780,#1704,.T.);
#3329=EDGE_CURVE('',#2785,#2785,#2422,.T.);
#3330=EDGE_CURVE('',#2785,#2786,#1705,.T.);
#3331=EDGE_CURVE('',#2786,#2786,#2423,.T.);
#3332=EDGE_CURVE('',#2787,#2787,#2424,.T.);
#3333=EDGE_CURVE('',#2788,#2788,#2425,.T.);
#3334=EDGE_CURVE('',#2788,#2789,#1706,.T.);
#3335=EDGE_CURVE('',#2789,#2789,#2426,.T.);
#3336=EDGE_CURVE('',#2790,#2790,#2427,.T.);
#3337=EDGE_CURVE('',#2777,#2772,#1707,.T.);
#3338=EDGE_CURVE('',#2773,#2776,#1708,.T.);
#3339=EDGE_CURVE('',#2791,#2791,#2428,.T.);
#3340=EDGE_CURVE('',#2791,#2787,#1709,.T.);
#3341=EDGE_CURVE('',#2792,#2792,#2429,.T.);
#3342=EDGE_CURVE('',#2792,#2790,#1710,.T.);
#3343=EDGE_CURVE('',#2793,#2793,#2430,.T.);
#3344=EDGE_CURVE('',#2793,#2781,#1711,.T.);
#3345=EDGE_CURVE('',#2783,#2794,#1712,.T.);
#3346=EDGE_CURVE('',#2794,#2794,#2431,.T.);
#3347=EDGE_CURVE('',#2770,#2775,#1713,.T.);
#3348=EDGE_CURVE('',#2771,#2774,#1714,.T.);
#3349=EDGE_CURVE('',#2795,#2796,#1715,.T.);
#3350=EDGE_CURVE('',#2795,#2797,#1716,.T.);
#3351=EDGE_CURVE('',#2797,#2798,#1717,.T.);
#3352=EDGE_CURVE('',#2796,#2798,#1718,.T.);
#3353=EDGE_CURVE('',#2799,#2795,#1719,.T.);
#3354=EDGE_CURVE('',#2799,#2800,#1720,.T.);
#3355=EDGE_CURVE('',#2800,#2797,#1721,.T.);
#3356=EDGE_CURVE('',#2801,#2799,#1722,.T.);
#3357=EDGE_CURVE('',#2801,#2802,#1723,.T.);
#3358=EDGE_CURVE('',#2802,#2800,#1724,.T.);
#3359=EDGE_CURVE('',#2803,#2801,#1725,.T.);
#3360=EDGE_CURVE('',#2803,#2804,#1726,.T.);
#3361=EDGE_CURVE('',#2804,#2802,#1727,.T.);
#3362=EDGE_CURVE('',#2805,#2803,#1728,.T.);
#3363=EDGE_CURVE('',#2805,#2806,#1729,.T.);
#3364=EDGE_CURVE('',#2806,#2804,#1730,.T.);
#3365=EDGE_CURVE('',#2796,#2805,#1731,.T.);
#3366=EDGE_CURVE('',#2798,#2806,#1732,.T.);
#3367=EDGE_CURVE('',#2807,#2807,#2432,.T.);
#3368=EDGE_CURVE('',#2808,#2808,#2433,.T.);
#3369=EDGE_CURVE('',#2808,#2807,#1733,.T.);
#3370=EDGE_CURVE('',#2809,#2809,#2434,.F.);
#3371=EDGE_CURVE('',#2809,#2808,#1734,.T.);
#3372=EDGE_CURVE('',#2810,#2810,#2435,.T.);
#3373=EDGE_CURVE('',#2810,#2809,#1735,.T.);
#3374=EDGE_CURVE('',#2811,#2811,#2436,.T.);
#3375=EDGE_CURVE('',#2811,#2812,#1736,.T.);
#3376=EDGE_CURVE('',#2812,#2812,#2437,.T.);
#3377=EDGE_CURVE('',#2813,#2813,#2438,.T.);
#3378=EDGE_CURVE('',#2813,#2814,#1737,.T.);
#3379=EDGE_CURVE('',#2814,#2814,#2439,.T.);
#3380=EDGE_CURVE('',#2815,#2815,#2440,.T.);
#3381=EDGE_CURVE('',#2815,#2816,#1738,.T.);
#3382=EDGE_CURVE('',#2816,#2816,#2441,.T.);
#3383=EDGE_CURVE('',#2817,#2818,#1739,.T.);
#3384=EDGE_CURVE('',#2817,#2819,#2442,.T.);
#3385=EDGE_CURVE('',#2820,#2819,#1740,.T.);
#3386=EDGE_CURVE('',#2818,#2820,#2443,.T.);
#3387=EDGE_CURVE('',#2821,#2818,#1741,.T.);
#3388=EDGE_CURVE('',#2822,#2821,#1742,.T.);
#3389=EDGE_CURVE('',#2817,#2822,#1743,.T.);
#3390=EDGE_CURVE('',#2820,#2823,#1744,.T.);
#3391=EDGE_CURVE('',#2823,#2824,#2444,.T.);
#3392=EDGE_CURVE('',#2824,#2825,#1745,.T.);
#3393=EDGE_CURVE('',#2825,#2826,#2445,.T.);
#3394=EDGE_CURVE('',#2826,#2827,#1746,.T.);
#3395=EDGE_CURVE('',#2827,#2828,#2446,.T.);
#3396=EDGE_CURVE('',#2828,#2829,#1747,.T.);
#3397=EDGE_CURVE('',#2829,#2830,#2447,.T.);
#3398=EDGE_CURVE('',#2830,#2831,#1748,.T.);
#3399=EDGE_CURVE('',#2831,#2821,#2448,.T.);
#3400=EDGE_CURVE('',#2832,#2819,#1749,.T.);
#3401=EDGE_CURVE('',#2823,#2832,#1750,.T.);
#3402=EDGE_CURVE('',#2831,#2833,#1751,.T.);
#3403=EDGE_CURVE('',#2833,#2822,#2449,.T.);
#3404=EDGE_CURVE('',#2832,#2834,#2450,.T.);
#3405=EDGE_CURVE('',#2834,#2824,#1752,.T.);
#3406=EDGE_CURVE('',#2826,#2835,#1753,.T.);
#3407=EDGE_CURVE('',#2836,#2825,#1754,.T.);
#3408=EDGE_CURVE('',#2836,#2835,#2451,.T.);
#3409=EDGE_CURVE('',#2837,#2835,#1755,.T.);
#3410=EDGE_CURVE('',#2827,#2837,#1756,.T.);
#3411=EDGE_CURVE('',#2833,#2838,#1757,.T.);
#3412=EDGE_CURVE('',#2839,#2838,#2452,.T.);
#3413=EDGE_CURVE('',#2839,#2840,#1758,.T.);
#3414=EDGE_CURVE('',#2837,#2840,#2453,.T.);
#3415=EDGE_CURVE('',#2836,#2834,#1759,.T.);
#3416=EDGE_CURVE('',#2841,#2841,#2454,.T.);
#3417=EDGE_CURVE('',#2839,#2829,#1760,.T.);
#3418=EDGE_CURVE('',#2830,#2838,#1761,.T.);
#3419=EDGE_CURVE('',#2840,#2828,#1762,.T.);
#3420=EDGE_CURVE('',#2842,#2842,#2455,.T.);
#3421=EDGE_CURVE('',#2843,#2843,#2456,.T.);
#3422=EDGE_CURVE('',#2841,#2842,#1763,.T.);
#3423=EDGE_CURVE('',#2843,#2844,#1764,.T.);
#3424=EDGE_CURVE('',#2844,#2844,#2457,.T.);
#3425=EDGE_CURVE('',#2845,#2845,#2458,.T.);
#3426=EDGE_CURVE('',#2845,#2846,#1765,.T.);
#3427=EDGE_CURVE('',#2846,#2846,#2459,.T.);
#3428=EDGE_CURVE('',#2847,#2847,#2460,.T.);
#3429=EDGE_CURVE('',#2847,#2848,#1766,.T.);
#3430=EDGE_CURVE('',#2848,#2848,#2461,.T.);
#3431=EDGE_CURVE('',#2849,#2849,#2462,.T.);
#3432=EDGE_CURVE('',#2849,#2850,#1767,.T.);
#3433=EDGE_CURVE('',#2850,#2850,#2463,.T.);
#3434=EDGE_CURVE('',#2851,#2851,#2464,.T.);
#3435=EDGE_CURVE('',#2851,#2852,#1768,.T.);
#3436=EDGE_CURVE('',#2852,#2852,#2465,.T.);
#3437=EDGE_CURVE('',#2853,#2854,#1769,.T.);
#3438=EDGE_CURVE('',#2853,#2854,#2466,.T.);
#3439=EDGE_CURVE('',#2855,#2853,#307,.T.);
#3440=EDGE_CURVE('',#2856,#2855,#2467,.T.);
#3441=EDGE_CURVE('',#2857,#2856,#308,.T.);
#3442=EDGE_CURVE('',#2857,#2858,#1770,.T.);
#3443=EDGE_CURVE('',#2859,#2858,#309,.T.);
#3444=EDGE_CURVE('',#2858,#2859,#310,.T.);
#3445=EDGE_CURVE('',#2854,#2857,#311,.T.);
#3446=EDGE_CURVE('',#2856,#2855,#1771,.T.);
#3447=EDGE_CURVE('',#2860,#2860,#2468,.T.);
#3448=EDGE_CURVE('',#2860,#2861,#1772,.T.);
#3449=EDGE_CURVE('',#2861,#2861,#2469,.T.);
#3450=EDGE_CURVE('',#2862,#2862,#2470,.T.);
#3451=EDGE_CURVE('',#2862,#2863,#1773,.T.);
#3452=EDGE_CURVE('',#2863,#2863,#2471,.T.);
#3453=EDGE_CURVE('',#2864,#2864,#2472,.T.);
#3454=EDGE_CURVE('',#2865,#2865,#2473,.T.);
#3455=EDGE_CURVE('',#2865,#2864,#1774,.T.);
#3456=EDGE_CURVE('',#2866,#2866,#2474,.T.);
#3457=EDGE_CURVE('',#2866,#2865,#1775,.T.);
#3458=EDGE_CURVE('',#2867,#2867,#2475,.T.);
#3459=EDGE_CURVE('',#2867,#2866,#1776,.T.);
#3460=EDGE_CURVE('',#2868,#2868,#2476,.T.);
#3461=EDGE_CURVE('',#2869,#2869,#2477,.F.);
#3462=EDGE_CURVE('',#2869,#2868,#1777,.T.);
#3463=EDGE_CURVE('',#2870,#2870,#2478,.F.);
#3464=EDGE_CURVE('',#2870,#2869,#1778,.T.);
#3465=EDGE_CURVE('',#2871,#2871,#2479,.T.);
#3466=EDGE_CURVE('',#2871,#2870,#1779,.T.);
#3467=EDGE_CURVE('',#2872,#2873,#1780,.T.);
#3468=EDGE_CURVE('',#2873,#2874,#1781,.T.);
#3469=EDGE_CURVE('',#2874,#2875,#1782,.T.);
#3470=EDGE_CURVE('',#2872,#2875,#1783,.T.);
#3471=EDGE_CURVE('',#2873,#2876,#1784,.T.);
#3472=EDGE_CURVE('',#2876,#2877,#1785,.T.);
#3473=EDGE_CURVE('',#2877,#2874,#1786,.T.);
#3474=EDGE_CURVE('',#2876,#2878,#1787,.T.);
#3475=EDGE_CURVE('',#2878,#2879,#1788,.T.);
#3476=EDGE_CURVE('',#2879,#2877,#1789,.T.);
#3477=EDGE_CURVE('',#2878,#2880,#1790,.T.);
#3478=EDGE_CURVE('',#2880,#2881,#1791,.T.);
#3479=EDGE_CURVE('',#2881,#2879,#1792,.T.);
#3480=EDGE_CURVE('',#2880,#2882,#1793,.T.);
#3481=EDGE_CURVE('',#2882,#2883,#1794,.T.);
#3482=EDGE_CURVE('',#2883,#2881,#1795,.T.);
#3483=EDGE_CURVE('',#2882,#2872,#1796,.T.);
#3484=EDGE_CURVE('',#2875,#2883,#1797,.T.);
#3485=EDGE_CURVE('',#2884,#2884,#2480,.T.);
#3486=EDGE_CURVE('',#2885,#2886,#1798,.T.);
#3487=EDGE_CURVE('',#2885,#2887,#1799,.T.);
#3488=EDGE_CURVE('',#2887,#2888,#1800,.T.);
#3489=EDGE_CURVE('',#2886,#2888,#1801,.T.);
#3490=EDGE_CURVE('',#2889,#2885,#1802,.T.);
#3491=EDGE_CURVE('',#2889,#2890,#1803,.T.);
#3492=EDGE_CURVE('',#2890,#2887,#1804,.T.);
#3493=EDGE_CURVE('',#2891,#2889,#1805,.T.);
#3494=EDGE_CURVE('',#2891,#2892,#1806,.T.);
#3495=EDGE_CURVE('',#2892,#2890,#1807,.T.);
#3496=EDGE_CURVE('',#2893,#2891,#1808,.T.);
#3497=EDGE_CURVE('',#2893,#2894,#1809,.T.);
#3498=EDGE_CURVE('',#2894,#2892,#1810,.T.);
#3499=EDGE_CURVE('',#2895,#2893,#1811,.T.);
#3500=EDGE_CURVE('',#2895,#2896,#1812,.T.);
#3501=EDGE_CURVE('',#2896,#2894,#1813,.T.);
#3502=EDGE_CURVE('',#2886,#2895,#1814,.T.);
#3503=EDGE_CURVE('',#2888,#2896,#1815,.T.);
#3504=EDGE_CURVE('',#2897,#2897,#2481,.T.);
#3505=EDGE_CURVE('',#2898,#2898,#2482,.T.);
#3506=EDGE_CURVE('',#2898,#2897,#1816,.T.);
#3507=EDGE_CURVE('',#2884,#2898,#1817,.T.);
#3508=EDGE_CURVE('',#2899,#2899,#2483,.T.);
#3509=EDGE_CURVE('',#2899,#2900,#1818,.T.);
#3510=EDGE_CURVE('',#2900,#2900,#2484,.T.);
#3511=EDGE_CURVE('',#2901,#2901,#2485,.T.);
#3512=EDGE_CURVE('',#2902,#2902,#2486,.T.);
#3513=EDGE_CURVE('',#2903,#2903,#2487,.T.);
#3514=EDGE_CURVE('',#2904,#2904,#2488,.T.);
#3515=EDGE_CURVE('',#2901,#2903,#1819,.T.);
#3516=EDGE_CURVE('',#2904,#2905,#1820,.T.);
#3517=EDGE_CURVE('',#2905,#2905,#2489,.T.);
#3518=EDGE_CURVE('',#2906,#2906,#2490,.T.);
#3519=EDGE_CURVE('',#2906,#2902,#1821,.T.);
#3520=EDGE_CURVE('',#2907,#2907,#2491,.T.);
#3521=EDGE_CURVE('',#2907,#2908,#1822,.T.);
#3522=EDGE_CURVE('',#2908,#2908,#2492,.T.);
#3523=EDGE_CURVE('',#2909,#2909,#2493,.T.);
#3524=EDGE_CURVE('',#2909,#2910,#1823,.T.);
#3525=EDGE_CURVE('',#2910,#2910,#2494,.T.);
#3526=EDGE_CURVE('',#2911,#2911,#2495,.T.);
#3527=EDGE_CURVE('',#2911,#2912,#1824,.T.);
#3528=EDGE_CURVE('',#2912,#2912,#2496,.T.);
#3529=EDGE_CURVE('',#2913,#2913,#2497,.T.);
#3530=EDGE_CURVE('',#2913,#2914,#1825,.T.);
#3531=EDGE_CURVE('',#2914,#2914,#2498,.T.);
#3532=EDGE_CURVE('',#2915,#2916,#1826,.T.);
#3533=EDGE_CURVE('',#2917,#2915,#2499,.T.);
#3534=EDGE_CURVE('',#2918,#2917,#1827,.T.);
#3535=EDGE_CURVE('',#2918,#2916,#2500,.T.);
#3536=EDGE_CURVE('',#2919,#2916,#1828,.T.);
#3537=EDGE_CURVE('',#2920,#2919,#1829,.T.);
#3538=EDGE_CURVE('',#2915,#2920,#1830,.T.);
#3539=EDGE_CURVE('',#2918,#2921,#1831,.T.);
#3540=EDGE_CURVE('',#2919,#2921,#2501,.T.);
#3541=EDGE_CURVE('',#2922,#2917,#1832,.T.);
#3542=EDGE_CURVE('',#2921,#2922,#1833,.T.);
#3543=EDGE_CURVE('',#2920,#2922,#2502,.T.);
#3544=EDGE_CURVE('',#2923,#2923,#2503,.T.);
#3545=EDGE_CURVE('',#2923,#2924,#1834,.T.);
#3546=EDGE_CURVE('',#2924,#2924,#2504,.T.);
#3547=EDGE_CURVE('',#2925,#2925,#2505,.T.);
#3548=EDGE_CURVE('',#2925,#2926,#1835,.T.);
#3549=EDGE_CURVE('',#2926,#2926,#2506,.T.);
#3550=EDGE_CURVE('',#2927,#2927,#2507,.T.);
#3551=EDGE_CURVE('',#2927,#2928,#1836,.T.);
#3552=EDGE_CURVE('',#2928,#2928,#2508,.T.);
#3553=EDGE_CURVE('',#2929,#2929,#2509,.T.);
#3554=EDGE_CURVE('',#2930,#2930,#2510,.T.);
#3555=EDGE_CURVE('',#2931,#2931,#2511,.T.);
#3556=EDGE_CURVE('',#2932,#2932,#2512,.T.);
#3557=EDGE_CURVE('',#2929,#2931,#1837,.T.);
#3558=EDGE_CURVE('',#2932,#2933,#1838,.T.);
#3559=EDGE_CURVE('',#2933,#2933,#2513,.T.);
#3560=EDGE_CURVE('',#2934,#2934,#2514,.T.);
#3561=EDGE_CURVE('',#2934,#2930,#1839,.T.);
#3562=EDGE_CURVE('',#2935,#2935,#2515,.T.);
#3563=EDGE_CURVE('',#2935,#2936,#1840,.T.);
#3564=EDGE_CURVE('',#2936,#2936,#2516,.T.);
#3565=EDGE_CURVE('',#2937,#2937,#2517,.T.);
#3566=EDGE_CURVE('',#2937,#2938,#1841,.T.);
#3567=EDGE_CURVE('',#2938,#2938,#2518,.T.);
#3568=EDGE_CURVE('',#2939,#2939,#2519,.T.);
#3569=EDGE_CURVE('',#2939,#2940,#1842,.T.);
#3570=EDGE_CURVE('',#2940,#2940,#2520,.T.);
#3571=EDGE_CURVE('',#2941,#2941,#2521,.T.);
#3572=EDGE_CURVE('',#2941,#2942,#1843,.T.);
#3573=EDGE_CURVE('',#2942,#2942,#2522,.T.);
#3574=EDGE_CURVE('',#2943,#2943,#2523,.T.);
#3575=EDGE_CURVE('',#2943,#2944,#1844,.T.);
#3576=EDGE_CURVE('',#2944,#2944,#2524,.T.);
#3577=EDGE_CURVE('',#2945,#2945,#2525,.T.);
#3578=EDGE_CURVE('',#2945,#2946,#1845,.T.);
#3579=EDGE_CURVE('',#2946,#2946,#2526,.T.);
#3580=EDGE_CURVE('',#2947,#2947,#2527,.T.);
#3581=EDGE_CURVE('',#2947,#2948,#1846,.T.);
#3582=EDGE_CURVE('',#2948,#2948,#2528,.T.);
#3583=EDGE_CURVE('',#2949,#2949,#2529,.T.);
#3584=EDGE_CURVE('',#2949,#2950,#1847,.T.);
#3585=EDGE_CURVE('',#2950,#2950,#2530,.T.);
#3586=EDGE_CURVE('',#2951,#2952,#1848,.T.);
#3587=EDGE_CURVE('',#2952,#2953,#1849,.T.);
#3588=EDGE_CURVE('',#2954,#2953,#1850,.T.);
#3589=EDGE_CURVE('',#2951,#2954,#1851,.T.);
#3590=EDGE_CURVE('',#2955,#2951,#1852,.T.);
#3591=EDGE_CURVE('',#2956,#2954,#1853,.T.);
#3592=EDGE_CURVE('',#2955,#2956,#1854,.T.);
#3593=EDGE_CURVE('',#2957,#2955,#1855,.T.);
#3594=EDGE_CURVE('',#2958,#2956,#1856,.T.);
#3595=EDGE_CURVE('',#2957,#2958,#1857,.T.);
#3596=EDGE_CURVE('',#2952,#2957,#1858,.T.);
#3597=EDGE_CURVE('',#2953,#2958,#1859,.T.);
#3598=EDGE_CURVE('',#2959,#2960,#2531,.T.);
#3599=EDGE_CURVE('',#2961,#2959,#1860,.T.);
#3600=EDGE_CURVE('',#2962,#2961,#1861,.T.);
#3601=EDGE_CURVE('',#2960,#2962,#1862,.T.);
#3602=EDGE_CURVE('',#2960,#2963,#1863,.T.);
#3603=EDGE_CURVE('',#2964,#2962,#1864,.T.);
#3604=EDGE_CURVE('',#2964,#2963,#1865,.T.);
#3605=EDGE_CURVE('',#2963,#2965,#2532,.T.);
#3606=EDGE_CURVE('',#2966,#2964,#1866,.T.);
#3607=EDGE_CURVE('',#2965,#2966,#1867,.T.);
#3608=EDGE_CURVE('',#2965,#2959,#1868,.T.);
#3609=EDGE_CURVE('',#2966,#2961,#1869,.T.);
#3610=EDGE_CURVE('',#2967,#2967,#2533,.T.);
#3611=EDGE_CURVE('',#2968,#2968,#2534,.T.);
#3612=EDGE_CURVE('',#2969,#2969,#2535,.T.);
#3613=EDGE_CURVE('',#2969,#2967,#1870,.T.);
#3614=EDGE_CURVE('',#2970,#2970,#2536,.T.);
#3615=EDGE_CURVE('',#2971,#2971,#2537,.T.);
#3616=EDGE_CURVE('',#2971,#2970,#1871,.T.);
#3617=EDGE_CURVE('',#2972,#2972,#2538,.T.);
#3618=EDGE_CURVE('',#2973,#2973,#2539,.T.);
#3619=EDGE_CURVE('',#2973,#2972,#1872,.T.);
#3620=EDGE_CURVE('',#2974,#2974,#2540,.T.);
#3621=EDGE_CURVE('',#2975,#2975,#2541,.T.);
#3622=EDGE_CURVE('',#2975,#2974,#1873,.T.);
#3623=EDGE_CURVE('',#2976,#2976,#2542,.T.);
#3624=EDGE_CURVE('',#2977,#2977,#2543,.T.);
#3625=EDGE_CURVE('',#2977,#2976,#1874,.T.);
#3626=EDGE_CURVE('',#2978,#2978,#2544,.T.);
#3627=EDGE_CURVE('',#2978,#2968,#1875,.T.);
#3628=EDGE_CURVE('',#2979,#2980,#2545,.T.);
#3629=EDGE_CURVE('',#2981,#2979,#1876,.T.);
#3630=EDGE_CURVE('',#2982,#2981,#2546,.T.);
#3631=EDGE_CURVE('',#2980,#2982,#1877,.T.);
#3632=EDGE_CURVE('',#2980,#2983,#1878,.T.);
#3633=EDGE_CURVE('',#2984,#2982,#1879,.T.);
#3634=EDGE_CURVE('',#2984,#2983,#1880,.T.);
#3635=EDGE_CURVE('',#2983,#2985,#2547,.T.);
#3636=EDGE_CURVE('',#2986,#2984,#2548,.T.);
#3637=EDGE_CURVE('',#2985,#2986,#1881,.T.);
#3638=EDGE_CURVE('',#2985,#2979,#1882,.T.);
#3639=EDGE_CURVE('',#2981,#2986,#1883,.T.);
#3640=EDGE_CURVE('',#2987,#2987,#2549,.T.);
#3641=EDGE_CURVE('',#2988,#2988,#2550,.T.);
#3642=EDGE_CURVE('',#2989,#2989,#2551,.T.);
#3643=EDGE_CURVE('',#2989,#2987,#1884,.T.);
#3644=EDGE_CURVE('',#2990,#2990,#2552,.T.);
#3645=EDGE_CURVE('',#2990,#2988,#1885,.T.);
#3646=EDGE_CURVE('',#2991,#2991,#2553,.T.);
#3647=EDGE_CURVE('',#2991,#2992,#1886,.T.);
#3648=EDGE_CURVE('',#2992,#2992,#2554,.T.);
#3649=EDGE_CURVE('',#2993,#2993,#2555,.T.);
#3650=EDGE_CURVE('',#2993,#2994,#1887,.T.);
#3651=EDGE_CURVE('',#2994,#2994,#2556,.T.);
#3652=EDGE_CURVE('',#2995,#2995,#2557,.T.);
#3653=EDGE_CURVE('',#2995,#2996,#1888,.T.);
#3654=EDGE_CURVE('',#2996,#2996,#2558,.T.);
#3655=EDGE_CURVE('',#2997,#2997,#2559,.T.);
#3656=EDGE_CURVE('',#2997,#2998,#1889,.T.);
#3657=EDGE_CURVE('',#2998,#2998,#2560,.T.);
#3658=EDGE_CURVE('',#2999,#2999,#2561,.T.);
#3659=EDGE_CURVE('',#2999,#3000,#1890,.T.);
#3660=EDGE_CURVE('',#3000,#3000,#2562,.T.);
#3661=EDGE_CURVE('',#3001,#3002,#1891,.T.);
#3662=EDGE_CURVE('',#3002,#3003,#1892,.T.);
#3663=EDGE_CURVE('',#3004,#3003,#1893,.T.);
#3664=EDGE_CURVE('',#3001,#3004,#1894,.T.);
#3665=EDGE_CURVE('',#3005,#3001,#1895,.T.);
#3666=EDGE_CURVE('',#3006,#3004,#1896,.T.);
#3667=EDGE_CURVE('',#3005,#3006,#1897,.T.);
#3668=EDGE_CURVE('',#3007,#3005,#1898,.T.);
#3669=EDGE_CURVE('',#3008,#3006,#1899,.T.);
#3670=EDGE_CURVE('',#3007,#3008,#1900,.T.);
#3671=EDGE_CURVE('',#3002,#3007,#1901,.T.);
#3672=EDGE_CURVE('',#3003,#3008,#1902,.T.);
#3673=EDGE_CURVE('',#3009,#3009,#2563,.T.);
#3674=EDGE_CURVE('',#3009,#3010,#1903,.T.);
#3675=EDGE_CURVE('',#3010,#3010,#2564,.T.);
#3676=EDGE_CURVE('',#3011,#3011,#2565,.T.);
#3677=EDGE_CURVE('',#3011,#3012,#1904,.T.);
#3678=EDGE_CURVE('',#3012,#3012,#2566,.T.);
#3679=EDGE_CURVE('',#3013,#3013,#2567,.T.);
#3680=EDGE_CURVE('',#3013,#3014,#1905,.T.);
#3681=EDGE_CURVE('',#3014,#3014,#2568,.T.);
#3682=EDGE_CURVE('',#3015,#3015,#2569,.T.);
#3683=EDGE_CURVE('',#3015,#3016,#1906,.T.);
#3684=EDGE_CURVE('',#3016,#3016,#2570,.T.);
#3685=EDGE_CURVE('',#3017,#3018,#1907,.T.);
#3686=EDGE_CURVE('',#3018,#3019,#1908,.T.);
#3687=EDGE_CURVE('',#3019,#3020,#1909,.T.);
#3688=EDGE_CURVE('',#3017,#3020,#1910,.T.);
#3689=EDGE_CURVE('',#3018,#3021,#1911,.T.);
#3690=EDGE_CURVE('',#3021,#3022,#1912,.T.);
#3691=EDGE_CURVE('',#3022,#3019,#1913,.T.);
#3692=EDGE_CURVE('',#3021,#3023,#1914,.T.);
#3693=EDGE_CURVE('',#3023,#3024,#1915,.T.);
#3694=EDGE_CURVE('',#3024,#3022,#1916,.T.);
#3695=EDGE_CURVE('',#3023,#3025,#1917,.T.);
#3696=EDGE_CURVE('',#3025,#3026,#1918,.T.);
#3697=EDGE_CURVE('',#3026,#3024,#1919,.T.);
#3698=EDGE_CURVE('',#3025,#3027,#1920,.T.);
#3699=EDGE_CURVE('',#3027,#3028,#1921,.T.);
#3700=EDGE_CURVE('',#3028,#3026,#1922,.T.);
#3701=EDGE_CURVE('',#3027,#3017,#1923,.T.);
#3702=EDGE_CURVE('',#3020,#3028,#1924,.T.);
#3703=EDGE_CURVE('',#3029,#3029,#2571,.T.);
#3704=EDGE_CURVE('',#3030,#3030,#2572,.T.);
#3705=EDGE_CURVE('',#3031,#3031,#2573,.T.);
#3706=EDGE_CURVE('',#3031,#3030,#1925,.T.);
#3707=EDGE_CURVE('',#3032,#3032,#2574,.T.);
#3708=EDGE_CURVE('',#3032,#3031,#1926,.T.);
#3709=EDGE_CURVE('',#3033,#3033,#2575,.T.);
#3710=EDGE_CURVE('',#3033,#3032,#1927,.T.);
#3711=EDGE_CURVE('',#3034,#3034,#2576,.T.);
#3712=EDGE_CURVE('',#3035,#3035,#2577,.F.);
#3713=EDGE_CURVE('',#3035,#3034,#1928,.T.);
#3714=EDGE_CURVE('',#3029,#3035,#1929,.T.);
#3715=ORIENTED_EDGE('',*,*,#3036,.F.);
#3716=ORIENTED_EDGE('',*,*,#3037,.T.);
#3717=ORIENTED_EDGE('',*,*,#3038,.F.);
#3718=ORIENTED_EDGE('',*,*,#3037,.F.);
#3719=ORIENTED_EDGE('',*,*,#3039,.F.);
#3720=ORIENTED_EDGE('',*,*,#3040,.T.);
#3721=ORIENTED_EDGE('',*,*,#3041,.F.);
#3722=ORIENTED_EDGE('',*,*,#3040,.F.);
#3723=ORIENTED_EDGE('',*,*,#3042,.F.);
#3724=ORIENTED_EDGE('',*,*,#3043,.T.);
#3725=ORIENTED_EDGE('',*,*,#3044,.F.);
#3726=ORIENTED_EDGE('',*,*,#3043,.F.);
#3727=ORIENTED_EDGE('',*,*,#3045,.F.);
#3728=ORIENTED_EDGE('',*,*,#3046,.T.);
#3729=ORIENTED_EDGE('',*,*,#3047,.F.);
#3730=ORIENTED_EDGE('',*,*,#3046,.F.);
#3731=ORIENTED_EDGE('',*,*,#3048,.F.);
#3732=ORIENTED_EDGE('',*,*,#3049,.T.);
#3733=ORIENTED_EDGE('',*,*,#3050,.F.);
#3734=ORIENTED_EDGE('',*,*,#3049,.F.);
#3735=ORIENTED_EDGE('',*,*,#3051,.F.);
#3736=ORIENTED_EDGE('',*,*,#3052,.T.);
#3737=ORIENTED_EDGE('',*,*,#3053,.F.);
#3738=ORIENTED_EDGE('',*,*,#3052,.F.);
#3739=ORIENTED_EDGE('',*,*,#3054,.F.);
#3740=ORIENTED_EDGE('',*,*,#3055,.T.);
#3741=ORIENTED_EDGE('',*,*,#3056,.F.);
#3742=ORIENTED_EDGE('',*,*,#3055,.F.);
#3743=ORIENTED_EDGE('',*,*,#3057,.F.);
#3744=ORIENTED_EDGE('',*,*,#3058,.T.);
#3745=ORIENTED_EDGE('',*,*,#3059,.F.);
#3746=ORIENTED_EDGE('',*,*,#3058,.F.);
#3747=ORIENTED_EDGE('',*,*,#3060,.T.);
#3748=ORIENTED_EDGE('',*,*,#3061,.T.);
#3749=ORIENTED_EDGE('',*,*,#3062,.F.);
#3750=ORIENTED_EDGE('',*,*,#3063,.F.);
#3751=ORIENTED_EDGE('',*,*,#3064,.T.);
#3752=ORIENTED_EDGE('',*,*,#3063,.T.);
#3753=ORIENTED_EDGE('',*,*,#3065,.F.);
#3754=ORIENTED_EDGE('',*,*,#3066,.F.);
#3755=ORIENTED_EDGE('',*,*,#3067,.T.);
#3756=ORIENTED_EDGE('',*,*,#3066,.T.);
#3757=ORIENTED_EDGE('',*,*,#3068,.F.);
#3758=ORIENTED_EDGE('',*,*,#3069,.F.);
#3759=ORIENTED_EDGE('',*,*,#3070,.T.);
#3760=ORIENTED_EDGE('',*,*,#3069,.T.);
#3761=ORIENTED_EDGE('',*,*,#3071,.F.);
#3762=ORIENTED_EDGE('',*,*,#3061,.F.);
#3763=ORIENTED_EDGE('',*,*,#3071,.T.);
#3764=ORIENTED_EDGE('',*,*,#3068,.T.);
#3765=ORIENTED_EDGE('',*,*,#3065,.T.);
#3766=ORIENTED_EDGE('',*,*,#3062,.T.);
#3767=ORIENTED_EDGE('',*,*,#3059,.T.);
#3768=ORIENTED_EDGE('',*,*,#3056,.T.);
#3769=ORIENTED_EDGE('',*,*,#3053,.T.);
#3770=ORIENTED_EDGE('',*,*,#3050,.T.);
#3771=ORIENTED_EDGE('',*,*,#3047,.T.);
#3772=ORIENTED_EDGE('',*,*,#3044,.T.);
#3773=ORIENTED_EDGE('',*,*,#3041,.T.);
#3774=ORIENTED_EDGE('',*,*,#3038,.T.);
#3775=ORIENTED_EDGE('',*,*,#3070,.F.);
#3776=ORIENTED_EDGE('',*,*,#3060,.F.);
#3777=ORIENTED_EDGE('',*,*,#3064,.F.);
#3778=ORIENTED_EDGE('',*,*,#3067,.F.);
#3779=ORIENTED_EDGE('',*,*,#3057,.T.);
#3780=ORIENTED_EDGE('',*,*,#3054,.T.);
#3781=ORIENTED_EDGE('',*,*,#3051,.T.);
#3782=ORIENTED_EDGE('',*,*,#3048,.T.);
#3783=ORIENTED_EDGE('',*,*,#3045,.T.);
#3784=ORIENTED_EDGE('',*,*,#3042,.T.);
#3785=ORIENTED_EDGE('',*,*,#3039,.T.);
#3786=ORIENTED_EDGE('',*,*,#3036,.T.);
#3787=ORIENTED_EDGE('',*,*,#3072,.T.);
#3788=ORIENTED_EDGE('',*,*,#3073,.T.);
#3789=ORIENTED_EDGE('',*,*,#3074,.T.);
#3790=ORIENTED_EDGE('',*,*,#3075,.F.);
#3791=ORIENTED_EDGE('',*,*,#3076,.T.);
#3792=ORIENTED_EDGE('',*,*,#3077,.T.);
#3793=ORIENTED_EDGE('',*,*,#3078,.T.);
#3794=ORIENTED_EDGE('',*,*,#3073,.F.);
#3795=ORIENTED_EDGE('',*,*,#3079,.T.);
#3796=ORIENTED_EDGE('',*,*,#3080,.T.);
#3797=ORIENTED_EDGE('',*,*,#3081,.T.);
#3798=ORIENTED_EDGE('',*,*,#3077,.F.);
#3799=ORIENTED_EDGE('',*,*,#3082,.T.);
#3800=ORIENTED_EDGE('',*,*,#3083,.T.);
#3801=ORIENTED_EDGE('',*,*,#3084,.T.);
#3802=ORIENTED_EDGE('',*,*,#3080,.F.);
#3803=ORIENTED_EDGE('',*,*,#3085,.T.);
#3804=ORIENTED_EDGE('',*,*,#3086,.T.);
#3805=ORIENTED_EDGE('',*,*,#3087,.T.);
#3806=ORIENTED_EDGE('',*,*,#3083,.F.);
#3807=ORIENTED_EDGE('',*,*,#3088,.T.);
#3808=ORIENTED_EDGE('',*,*,#3075,.T.);
#3809=ORIENTED_EDGE('',*,*,#3089,.T.);
#3810=ORIENTED_EDGE('',*,*,#3086,.F.);
#3811=ORIENTED_EDGE('',*,*,#3088,.F.);
#3812=ORIENTED_EDGE('',*,*,#3085,.F.);
#3813=ORIENTED_EDGE('',*,*,#3082,.F.);
#3814=ORIENTED_EDGE('',*,*,#3079,.F.);
#3815=ORIENTED_EDGE('',*,*,#3076,.F.);
#3816=ORIENTED_EDGE('',*,*,#3072,.F.);
#3817=ORIENTED_EDGE('',*,*,#3089,.F.);
#3818=ORIENTED_EDGE('',*,*,#3074,.F.);
#3819=ORIENTED_EDGE('',*,*,#3078,.F.);
#3820=ORIENTED_EDGE('',*,*,#3081,.F.);
#3821=ORIENTED_EDGE('',*,*,#3084,.F.);
#3822=ORIENTED_EDGE('',*,*,#3087,.F.);
#3823=ORIENTED_EDGE('',*,*,#3090,.F.);
#3824=ORIENTED_EDGE('',*,*,#3091,.F.);
#3825=ORIENTED_EDGE('',*,*,#3092,.F.);
#3826=ORIENTED_EDGE('',*,*,#3093,.T.);
#3827=ORIENTED_EDGE('',*,*,#3091,.T.);
#3828=ORIENTED_EDGE('',*,*,#3093,.F.);
#3829=ORIENTED_EDGE('',*,*,#3094,.F.);
#3830=ORIENTED_EDGE('',*,*,#3095,.T.);
#3831=ORIENTED_EDGE('',*,*,#3092,.T.);
#3832=ORIENTED_EDGE('',*,*,#3095,.F.);
#3833=ORIENTED_EDGE('',*,*,#3096,.F.);
#3834=ORIENTED_EDGE('',*,*,#3097,.T.);
#3835=ORIENTED_EDGE('',*,*,#3094,.T.);
#3836=ORIENTED_EDGE('',*,*,#3097,.F.);
#3837=ORIENTED_EDGE('',*,*,#3096,.T.);
#3838=ORIENTED_EDGE('',*,*,#3098,.F.);
#3839=ORIENTED_EDGE('',*,*,#3099,.F.);
#3840=ORIENTED_EDGE('',*,*,#3100,.T.);
#3841=ORIENTED_EDGE('',*,*,#3098,.T.);
#3842=ORIENTED_EDGE('',*,*,#3100,.F.);
#3843=ORIENTED_EDGE('',*,*,#3090,.T.);
#3844=ORIENTED_EDGE('',*,*,#3101,.T.);
#3845=ORIENTED_EDGE('',*,*,#3099,.T.);
#3846=ORIENTED_EDGE('',*,*,#3101,.F.);
#3847=ORIENTED_EDGE('',*,*,#3102,.F.);
#3848=ORIENTED_EDGE('',*,*,#3103,.F.);
#3849=ORIENTED_EDGE('',*,*,#3104,.T.);
#3850=ORIENTED_EDGE('',*,*,#3105,.F.);
#3851=ORIENTED_EDGE('',*,*,#3106,.F.);
#3852=ORIENTED_EDGE('',*,*,#3104,.F.);
#3853=ORIENTED_EDGE('',*,*,#3107,.F.);
#3854=ORIENTED_EDGE('',*,*,#3108,.T.);
#3855=ORIENTED_EDGE('',*,*,#3109,.F.);
#3856=ORIENTED_EDGE('',*,*,#3108,.F.);
#3857=ORIENTED_EDGE('',*,*,#3107,.T.);
#3858=ORIENTED_EDGE('',*,*,#3110,.F.);
#3859=ORIENTED_EDGE('',*,*,#3111,.T.);
#3860=ORIENTED_EDGE('',*,*,#3112,.F.);
#3861=ORIENTED_EDGE('',*,*,#3111,.F.);
#3862=ORIENTED_EDGE('',*,*,#3110,.T.);
#3863=ORIENTED_EDGE('',*,*,#3113,.F.);
#3864=ORIENTED_EDGE('',*,*,#3114,.T.);
#3865=ORIENTED_EDGE('',*,*,#3115,.F.);
#3866=ORIENTED_EDGE('',*,*,#3114,.F.);
#3867=ORIENTED_EDGE('',*,*,#3113,.T.);
#3868=ORIENTED_EDGE('',*,*,#3116,.F.);
#3869=ORIENTED_EDGE('',*,*,#3117,.T.);
#3870=ORIENTED_EDGE('',*,*,#3118,.F.);
#3871=ORIENTED_EDGE('',*,*,#3117,.F.);
#3872=ORIENTED_EDGE('',*,*,#3116,.T.);
#3873=ORIENTED_EDGE('',*,*,#3119,.F.);
#3874=ORIENTED_EDGE('',*,*,#3120,.F.);
#3875=ORIENTED_EDGE('',*,*,#3121,.F.);
#3876=ORIENTED_EDGE('',*,*,#3122,.F.);
#3877=ORIENTED_EDGE('',*,*,#3123,.F.);
#3878=ORIENTED_EDGE('',*,*,#3120,.T.);
#3879=ORIENTED_EDGE('',*,*,#3124,.F.);
#3880=ORIENTED_EDGE('',*,*,#3125,.T.);
#3881=ORIENTED_EDGE('',*,*,#3126,.F.);
#3882=ORIENTED_EDGE('',*,*,#3127,.F.);
#3883=ORIENTED_EDGE('',*,*,#3128,.F.);
#3884=ORIENTED_EDGE('',*,*,#3125,.F.);
#3885=ORIENTED_EDGE('',*,*,#3129,.F.);
#3886=ORIENTED_EDGE('',*,*,#3130,.T.);
#3887=ORIENTED_EDGE('',*,*,#3131,.F.);
#3888=ORIENTED_EDGE('',*,*,#3132,.F.);
#3889=ORIENTED_EDGE('',*,*,#3133,.F.);
#3890=ORIENTED_EDGE('',*,*,#3130,.F.);
#3891=ORIENTED_EDGE('',*,*,#3134,.F.);
#3892=ORIENTED_EDGE('',*,*,#3135,.T.);
#3893=ORIENTED_EDGE('',*,*,#3136,.F.);
#3894=ORIENTED_EDGE('',*,*,#3137,.F.);
#3895=ORIENTED_EDGE('',*,*,#3138,.F.);
#3896=ORIENTED_EDGE('',*,*,#3135,.F.);
#3897=ORIENTED_EDGE('',*,*,#3139,.F.);
#3898=ORIENTED_EDGE('',*,*,#3140,.T.);
#3899=ORIENTED_EDGE('',*,*,#3141,.T.);
#3900=ORIENTED_EDGE('',*,*,#3121,.T.);
#3901=ORIENTED_EDGE('',*,*,#3119,.T.);
#3902=ORIENTED_EDGE('',*,*,#3123,.T.);
#3903=ORIENTED_EDGE('',*,*,#3142,.T.);
#3904=ORIENTED_EDGE('',*,*,#3136,.T.);
#3905=ORIENTED_EDGE('',*,*,#3138,.T.);
#3906=ORIENTED_EDGE('',*,*,#3134,.T.);
#3907=ORIENTED_EDGE('',*,*,#3143,.T.);
#3908=ORIENTED_EDGE('',*,*,#3131,.T.);
#3909=ORIENTED_EDGE('',*,*,#3133,.T.);
#3910=ORIENTED_EDGE('',*,*,#3129,.T.);
#3911=ORIENTED_EDGE('',*,*,#3144,.T.);
#3912=ORIENTED_EDGE('',*,*,#3126,.T.);
#3913=ORIENTED_EDGE('',*,*,#3128,.T.);
#3914=ORIENTED_EDGE('',*,*,#3124,.T.);
#3915=ORIENTED_EDGE('',*,*,#3145,.T.);
#3916=ORIENTED_EDGE('',*,*,#3140,.F.);
#3917=ORIENTED_EDGE('',*,*,#3146,.T.);
#3918=ORIENTED_EDGE('',*,*,#3145,.F.);
#3919=ORIENTED_EDGE('',*,*,#3127,.T.);
#3920=ORIENTED_EDGE('',*,*,#3144,.F.);
#3921=ORIENTED_EDGE('',*,*,#3132,.T.);
#3922=ORIENTED_EDGE('',*,*,#3143,.F.);
#3923=ORIENTED_EDGE('',*,*,#3137,.T.);
#3924=ORIENTED_EDGE('',*,*,#3142,.F.);
#3925=ORIENTED_EDGE('',*,*,#3122,.T.);
#3926=ORIENTED_EDGE('',*,*,#3141,.F.);
#3927=ORIENTED_EDGE('',*,*,#3147,.T.);
#3928=ORIENTED_EDGE('',*,*,#3148,.T.);
#3929=ORIENTED_EDGE('',*,*,#3149,.T.);
#3930=ORIENTED_EDGE('',*,*,#3150,.T.);
#3931=ORIENTED_EDGE('',*,*,#3151,.F.);
#3932=ORIENTED_EDGE('',*,*,#3152,.T.);
#3933=ORIENTED_EDGE('',*,*,#3147,.F.);
#3934=ORIENTED_EDGE('',*,*,#3152,.F.);
#3935=ORIENTED_EDGE('',*,*,#3153,.F.);
#3936=ORIENTED_EDGE('',*,*,#3154,.T.);
#3937=ORIENTED_EDGE('',*,*,#3150,.F.);
#3938=ORIENTED_EDGE('',*,*,#3154,.F.);
#3939=ORIENTED_EDGE('',*,*,#3155,.F.);
#3940=ORIENTED_EDGE('',*,*,#3156,.T.);
#3941=ORIENTED_EDGE('',*,*,#3148,.F.);
#3942=ORIENTED_EDGE('',*,*,#3156,.F.);
#3943=ORIENTED_EDGE('',*,*,#3157,.F.);
#3944=ORIENTED_EDGE('',*,*,#3158,.T.);
#3945=ORIENTED_EDGE('',*,*,#3149,.F.);
#3946=ORIENTED_EDGE('',*,*,#3158,.F.);
#3947=ORIENTED_EDGE('',*,*,#3159,.F.);
#3948=ORIENTED_EDGE('',*,*,#3160,.T.);
#3949=ORIENTED_EDGE('',*,*,#3161,.F.);
#3950=ORIENTED_EDGE('',*,*,#3160,.F.);
#3951=ORIENTED_EDGE('',*,*,#3159,.T.);
#3952=ORIENTED_EDGE('',*,*,#3162,.F.);
#3953=ORIENTED_EDGE('',*,*,#3146,.F.);
#3954=ORIENTED_EDGE('',*,*,#3163,.T.);
#3955=ORIENTED_EDGE('',*,*,#3164,.T.);
#3956=ORIENTED_EDGE('',*,*,#3163,.F.);
#3957=ORIENTED_EDGE('',*,*,#3105,.T.);
#3958=ORIENTED_EDGE('',*,*,#3106,.T.);
#3959=ORIENTED_EDGE('',*,*,#3162,.T.);
#3960=ORIENTED_EDGE('',*,*,#3165,.T.);
#3961=ORIENTED_EDGE('',*,*,#3166,.T.);
#3962=ORIENTED_EDGE('',*,*,#3165,.F.);
#3963=ORIENTED_EDGE('',*,*,#3102,.T.);
#3964=ORIENTED_EDGE('',*,*,#3103,.T.);
#3965=ORIENTED_EDGE('',*,*,#3139,.T.);
#3966=ORIENTED_EDGE('',*,*,#3161,.T.);
#3967=ORIENTED_EDGE('',*,*,#3118,.T.);
#3968=ORIENTED_EDGE('',*,*,#3115,.T.);
#3969=ORIENTED_EDGE('',*,*,#3112,.T.);
#3970=ORIENTED_EDGE('',*,*,#3109,.T.);
#3971=ORIENTED_EDGE('',*,*,#3164,.F.);
#3972=ORIENTED_EDGE('',*,*,#3166,.F.);
#3973=ORIENTED_EDGE('',*,*,#3157,.T.);
#3974=ORIENTED_EDGE('',*,*,#3155,.T.);
#3975=ORIENTED_EDGE('',*,*,#3153,.T.);
#3976=ORIENTED_EDGE('',*,*,#3151,.T.);
#3977=ORIENTED_EDGE('',*,*,#3167,.F.);
#3978=ORIENTED_EDGE('',*,*,#3168,.T.);
#3979=ORIENTED_EDGE('',*,*,#3169,.F.);
#3980=ORIENTED_EDGE('',*,*,#3168,.F.);
#3981=ORIENTED_EDGE('',*,*,#3167,.T.);
#3982=ORIENTED_EDGE('',*,*,#3170,.F.);
#3983=ORIENTED_EDGE('',*,*,#3171,.F.);
#3984=ORIENTED_EDGE('',*,*,#3172,.T.);
#3985=ORIENTED_EDGE('',*,*,#3173,.F.);
#3986=ORIENTED_EDGE('',*,*,#3172,.F.);
#3987=ORIENTED_EDGE('',*,*,#3171,.T.);
#3988=ORIENTED_EDGE('',*,*,#3174,.F.);
#3989=ORIENTED_EDGE('',*,*,#3175,.F.);
#3990=ORIENTED_EDGE('',*,*,#3176,.T.);
#3991=ORIENTED_EDGE('',*,*,#3177,.F.);
#3992=ORIENTED_EDGE('',*,*,#3176,.F.);
#3993=ORIENTED_EDGE('',*,*,#3175,.T.);
#3994=ORIENTED_EDGE('',*,*,#3178,.F.);
#3995=ORIENTED_EDGE('',*,*,#3179,.F.);
#3996=ORIENTED_EDGE('',*,*,#3180,.T.);
#3997=ORIENTED_EDGE('',*,*,#3181,.F.);
#3998=ORIENTED_EDGE('',*,*,#3180,.F.);
#3999=ORIENTED_EDGE('',*,*,#3179,.T.);
#4000=ORIENTED_EDGE('',*,*,#3182,.F.);
#4001=ORIENTED_EDGE('',*,*,#3183,.F.);
#4002=ORIENTED_EDGE('',*,*,#3184,.T.);
#4003=ORIENTED_EDGE('',*,*,#3170,.T.);
#4004=ORIENTED_EDGE('',*,*,#3184,.F.);
#4005=ORIENTED_EDGE('',*,*,#3185,.F.);
#4006=ORIENTED_EDGE('',*,*,#3186,.T.);
#4007=ORIENTED_EDGE('',*,*,#3174,.T.);
#4008=ORIENTED_EDGE('',*,*,#3186,.F.);
#4009=ORIENTED_EDGE('',*,*,#3187,.F.);
#4010=ORIENTED_EDGE('',*,*,#3188,.T.);
#4011=ORIENTED_EDGE('',*,*,#3178,.T.);
#4012=ORIENTED_EDGE('',*,*,#3188,.F.);
#4013=ORIENTED_EDGE('',*,*,#3189,.F.);
#4014=ORIENTED_EDGE('',*,*,#3190,.T.);
#4015=ORIENTED_EDGE('',*,*,#3182,.T.);
#4016=ORIENTED_EDGE('',*,*,#3190,.F.);
#4017=ORIENTED_EDGE('',*,*,#3191,.F.);
#4018=ORIENTED_EDGE('',*,*,#3192,.T.);
#4019=ORIENTED_EDGE('',*,*,#3193,.T.);
#4020=ORIENTED_EDGE('',*,*,#3192,.F.);
#4021=ORIENTED_EDGE('',*,*,#3193,.F.);
#4022=ORIENTED_EDGE('',*,*,#3194,.F.);
#4023=ORIENTED_EDGE('',*,*,#3195,.F.);
#4024=ORIENTED_EDGE('',*,*,#3196,.T.);
#4025=ORIENTED_EDGE('',*,*,#3194,.T.);
#4026=ORIENTED_EDGE('',*,*,#3196,.F.);
#4027=ORIENTED_EDGE('',*,*,#3197,.F.);
#4028=ORIENTED_EDGE('',*,*,#3198,.T.);
#4029=ORIENTED_EDGE('',*,*,#3199,.T.);
#4030=ORIENTED_EDGE('',*,*,#3198,.F.);
#4031=ORIENTED_EDGE('',*,*,#3197,.T.);
#4032=ORIENTED_EDGE('',*,*,#3195,.T.);
#4033=ORIENTED_EDGE('',*,*,#3181,.T.);
#4034=ORIENTED_EDGE('',*,*,#3177,.T.);
#4035=ORIENTED_EDGE('',*,*,#3173,.T.);
#4036=ORIENTED_EDGE('',*,*,#3169,.T.);
#4037=ORIENTED_EDGE('',*,*,#3199,.F.);
#4038=ORIENTED_EDGE('',*,*,#3191,.T.);
#4039=ORIENTED_EDGE('',*,*,#3189,.T.);
#4040=ORIENTED_EDGE('',*,*,#3187,.T.);
#4041=ORIENTED_EDGE('',*,*,#3185,.T.);
#4042=ORIENTED_EDGE('',*,*,#3183,.T.);
#4043=ORIENTED_EDGE('',*,*,#3200,.F.);
#4044=ORIENTED_EDGE('',*,*,#3201,.F.);
#4045=ORIENTED_EDGE('',*,*,#3202,.T.);
#4046=ORIENTED_EDGE('',*,*,#3203,.F.);
#4047=ORIENTED_EDGE('',*,*,#3204,.F.);
#4048=ORIENTED_EDGE('',*,*,#3202,.F.);
#4049=ORIENTED_EDGE('',*,*,#3203,.T.);
#4050=ORIENTED_EDGE('',*,*,#3204,.T.);
#4051=ORIENTED_EDGE('',*,*,#3205,.T.);
#4052=ORIENTED_EDGE('',*,*,#3206,.T.);
#4053=ORIENTED_EDGE('',*,*,#3205,.F.);
#4054=ORIENTED_EDGE('',*,*,#3207,.T.);
#4055=ORIENTED_EDGE('',*,*,#3208,.T.);
#4056=ORIENTED_EDGE('',*,*,#3209,.F.);
#4057=ORIENTED_EDGE('',*,*,#3208,.F.);
#4058=ORIENTED_EDGE('',*,*,#3209,.T.);
#4059=ORIENTED_EDGE('',*,*,#3210,.T.);
#4060=ORIENTED_EDGE('',*,*,#3211,.F.);
#4061=ORIENTED_EDGE('',*,*,#3210,.F.);
#4062=ORIENTED_EDGE('',*,*,#3206,.F.);
#4063=ORIENTED_EDGE('',*,*,#3211,.T.);
#4064=ORIENTED_EDGE('',*,*,#3212,.F.);
#4065=ORIENTED_EDGE('',*,*,#3213,.T.);
#4066=ORIENTED_EDGE('',*,*,#3200,.T.);
#4067=ORIENTED_EDGE('',*,*,#3201,.T.);
#4068=ORIENTED_EDGE('',*,*,#3213,.F.);
#4069=ORIENTED_EDGE('',*,*,#3212,.T.);
#4070=ORIENTED_EDGE('',*,*,#3214,.F.);
#4071=ORIENTED_EDGE('',*,*,#3214,.T.);
#4072=ORIENTED_EDGE('',*,*,#3215,.T.);
#4073=ORIENTED_EDGE('',*,*,#3207,.F.);
#4074=ORIENTED_EDGE('',*,*,#3215,.F.);
#4075=ORIENTED_EDGE('',*,*,#3216,.F.);
#4076=ORIENTED_EDGE('',*,*,#3217,.F.);
#4077=ORIENTED_EDGE('',*,*,#3218,.T.);
#4078=ORIENTED_EDGE('',*,*,#3219,.F.);
#4079=ORIENTED_EDGE('',*,*,#3220,.F.);
#4080=ORIENTED_EDGE('',*,*,#3218,.F.);
#4081=ORIENTED_EDGE('',*,*,#3221,.T.);
#4082=ORIENTED_EDGE('',*,*,#3222,.T.);
#4083=ORIENTED_EDGE('',*,*,#3219,.T.);
#4084=ORIENTED_EDGE('',*,*,#3220,.T.);
#4085=ORIENTED_EDGE('',*,*,#3222,.F.);
#4086=ORIENTED_EDGE('',*,*,#3223,.F.);
#4087=ORIENTED_EDGE('',*,*,#3224,.T.);
#4088=ORIENTED_EDGE('',*,*,#3225,.F.);
#4089=ORIENTED_EDGE('',*,*,#3226,.T.);
#4090=ORIENTED_EDGE('',*,*,#3223,.T.);
#4091=ORIENTED_EDGE('',*,*,#3226,.F.);
#4092=ORIENTED_EDGE('',*,*,#3227,.F.);
#4093=ORIENTED_EDGE('',*,*,#3228,.T.);
#4094=ORIENTED_EDGE('',*,*,#3225,.T.);
#4095=ORIENTED_EDGE('',*,*,#3228,.F.);
#4096=ORIENTED_EDGE('',*,*,#3229,.F.);
#4097=ORIENTED_EDGE('',*,*,#3230,.T.);
#4098=ORIENTED_EDGE('',*,*,#3227,.T.);
#4099=ORIENTED_EDGE('',*,*,#3230,.F.);
#4100=ORIENTED_EDGE('',*,*,#3229,.T.);
#4101=ORIENTED_EDGE('',*,*,#3221,.F.);
#4102=ORIENTED_EDGE('',*,*,#3216,.T.);
#4103=ORIENTED_EDGE('',*,*,#3217,.T.);
#4104=ORIENTED_EDGE('',*,*,#3231,.T.);
#4105=ORIENTED_EDGE('',*,*,#3224,.F.);
#4106=ORIENTED_EDGE('',*,*,#3231,.F.);
#4107=ORIENTED_EDGE('',*,*,#3232,.T.);
#4108=ORIENTED_EDGE('',*,*,#3232,.F.);
#4109=ORIENTED_EDGE('',*,*,#3233,.T.);
#4110=ORIENTED_EDGE('',*,*,#3233,.F.);
#4111=ORIENTED_EDGE('',*,*,#3234,.T.);
#4112=ORIENTED_EDGE('',*,*,#3234,.F.);
#4113=ORIENTED_EDGE('',*,*,#3235,.T.);
#4114=ORIENTED_EDGE('',*,*,#3235,.F.);
#4115=ORIENTED_EDGE('',*,*,#3236,.T.);
#4116=ORIENTED_EDGE('',*,*,#3236,.F.);
#4117=ORIENTED_EDGE('',*,*,#3237,.T.);
#4118=ORIENTED_EDGE('',*,*,#3237,.F.);
#4119=ORIENTED_EDGE('',*,*,#3238,.T.);
#4120=ORIENTED_EDGE('',*,*,#3238,.F.);
#4121=ORIENTED_EDGE('',*,*,#3239,.T.);
#4122=ORIENTED_EDGE('',*,*,#3239,.F.);
#4123=ORIENTED_EDGE('',*,*,#3240,.F.);
#4124=ORIENTED_EDGE('',*,*,#3241,.F.);
#4125=ORIENTED_EDGE('',*,*,#3242,.F.);
#4126=ORIENTED_EDGE('',*,*,#3243,.F.);
#4127=ORIENTED_EDGE('',*,*,#3242,.T.);
#4128=ORIENTED_EDGE('',*,*,#3244,.F.);
#4129=ORIENTED_EDGE('',*,*,#3245,.T.);
#4130=ORIENTED_EDGE('',*,*,#3246,.F.);
#4131=ORIENTED_EDGE('',*,*,#3247,.T.);
#4132=ORIENTED_EDGE('',*,*,#3248,.F.);
#4133=ORIENTED_EDGE('',*,*,#3249,.T.);
#4134=ORIENTED_EDGE('',*,*,#3250,.T.);
#4135=ORIENTED_EDGE('',*,*,#3251,.F.);
#4136=ORIENTED_EDGE('',*,*,#3250,.F.);
#4137=ORIENTED_EDGE('',*,*,#3252,.T.);
#4138=ORIENTED_EDGE('',*,*,#3253,.F.);
#4139=ORIENTED_EDGE('',*,*,#3254,.T.);
#4140=ORIENTED_EDGE('',*,*,#3255,.F.);
#4141=ORIENTED_EDGE('',*,*,#3256,.T.);
#4142=ORIENTED_EDGE('',*,*,#3257,.F.);
#4143=ORIENTED_EDGE('',*,*,#3258,.T.);
#4144=ORIENTED_EDGE('',*,*,#3259,.F.);
#4145=ORIENTED_EDGE('',*,*,#3260,.T.);
#4146=ORIENTED_EDGE('',*,*,#3261,.F.);
#4147=ORIENTED_EDGE('',*,*,#3241,.T.);
#4148=ORIENTED_EDGE('',*,*,#3262,.T.);
#4149=ORIENTED_EDGE('',*,*,#3263,.T.);
#4150=ORIENTED_EDGE('',*,*,#3244,.T.);
#4151=ORIENTED_EDGE('',*,*,#3264,.F.);
#4152=ORIENTED_EDGE('',*,*,#3265,.F.);
#4153=ORIENTED_EDGE('',*,*,#3245,.F.);
#4154=ORIENTED_EDGE('',*,*,#3263,.F.);
#4155=ORIENTED_EDGE('',*,*,#3265,.T.);
#4156=ORIENTED_EDGE('',*,*,#3266,.T.);
#4157=ORIENTED_EDGE('',*,*,#3267,.T.);
#4158=ORIENTED_EDGE('',*,*,#3246,.T.);
#4159=ORIENTED_EDGE('',*,*,#3268,.F.);
#4160=ORIENTED_EDGE('',*,*,#3269,.F.);
#4161=ORIENTED_EDGE('',*,*,#3247,.F.);
#4162=ORIENTED_EDGE('',*,*,#3267,.F.);
#4163=ORIENTED_EDGE('',*,*,#3269,.T.);
#4164=ORIENTED_EDGE('',*,*,#3270,.T.);
#4165=ORIENTED_EDGE('',*,*,#3271,.T.);
#4166=ORIENTED_EDGE('',*,*,#3248,.T.);
#4167=ORIENTED_EDGE('',*,*,#3272,.F.);
#4168=ORIENTED_EDGE('',*,*,#3273,.F.);
#4169=ORIENTED_EDGE('',*,*,#3252,.F.);
#4170=ORIENTED_EDGE('',*,*,#3249,.F.);
#4171=ORIENTED_EDGE('',*,*,#3271,.F.);
#4172=ORIENTED_EDGE('',*,*,#3274,.F.);
#4173=ORIENTED_EDGE('',*,*,#3273,.T.);
#4174=ORIENTED_EDGE('',*,*,#3275,.T.);
#4175=ORIENTED_EDGE('',*,*,#3276,.T.);
#4176=ORIENTED_EDGE('',*,*,#3253,.T.);
#4177=ORIENTED_EDGE('',*,*,#3277,.F.);
#4178=ORIENTED_EDGE('',*,*,#3278,.F.);
#4179=ORIENTED_EDGE('',*,*,#3254,.F.);
#4180=ORIENTED_EDGE('',*,*,#3276,.F.);
#4181=ORIENTED_EDGE('',*,*,#3278,.T.);
#4182=ORIENTED_EDGE('',*,*,#3279,.T.);
#4183=ORIENTED_EDGE('',*,*,#3280,.T.);
#4184=ORIENTED_EDGE('',*,*,#3255,.T.);
#4185=ORIENTED_EDGE('',*,*,#3281,.F.);
#4186=ORIENTED_EDGE('',*,*,#3282,.F.);
#4187=ORIENTED_EDGE('',*,*,#3256,.F.);
#4188=ORIENTED_EDGE('',*,*,#3280,.F.);
#4189=ORIENTED_EDGE('',*,*,#3282,.T.);
#4190=ORIENTED_EDGE('',*,*,#3283,.T.);
#4191=ORIENTED_EDGE('',*,*,#3284,.T.);
#4192=ORIENTED_EDGE('',*,*,#3257,.T.);
#4193=ORIENTED_EDGE('',*,*,#3258,.F.);
#4194=ORIENTED_EDGE('',*,*,#3284,.F.);
#4195=ORIENTED_EDGE('',*,*,#3285,.F.);
#4196=ORIENTED_EDGE('',*,*,#3286,.F.);
#4197=ORIENTED_EDGE('',*,*,#3287,.F.);
#4198=ORIENTED_EDGE('',*,*,#3288,.T.);
#4199=ORIENTED_EDGE('',*,*,#3274,.T.);
#4200=ORIENTED_EDGE('',*,*,#3270,.F.);
#4201=ORIENTED_EDGE('',*,*,#3268,.T.);
#4202=ORIENTED_EDGE('',*,*,#3266,.F.);
#4203=ORIENTED_EDGE('',*,*,#3264,.T.);
#4204=ORIENTED_EDGE('',*,*,#3262,.F.);
#4205=ORIENTED_EDGE('',*,*,#3240,.T.);
#4206=ORIENTED_EDGE('',*,*,#3289,.F.);
#4207=ORIENTED_EDGE('',*,*,#3290,.T.);
#4208=ORIENTED_EDGE('',*,*,#3291,.F.);
#4209=ORIENTED_EDGE('',*,*,#3285,.T.);
#4210=ORIENTED_EDGE('',*,*,#3283,.F.);
#4211=ORIENTED_EDGE('',*,*,#3281,.T.);
#4212=ORIENTED_EDGE('',*,*,#3279,.F.);
#4213=ORIENTED_EDGE('',*,*,#3277,.T.);
#4214=ORIENTED_EDGE('',*,*,#3275,.F.);
#4215=ORIENTED_EDGE('',*,*,#3272,.T.);
#4216=ORIENTED_EDGE('',*,*,#3288,.F.);
#4217=ORIENTED_EDGE('',*,*,#3243,.T.);
#4218=ORIENTED_EDGE('',*,*,#3261,.T.);
#4219=ORIENTED_EDGE('',*,*,#3292,.T.);
#4220=ORIENTED_EDGE('',*,*,#3289,.T.);
#4221=ORIENTED_EDGE('',*,*,#3260,.F.);
#4222=ORIENTED_EDGE('',*,*,#3293,.F.);
#4223=ORIENTED_EDGE('',*,*,#3290,.F.);
#4224=ORIENTED_EDGE('',*,*,#3292,.F.);
#4225=ORIENTED_EDGE('',*,*,#3251,.T.);
#4226=ORIENTED_EDGE('',*,*,#3287,.T.);
#4227=ORIENTED_EDGE('',*,*,#3286,.T.);
#4228=ORIENTED_EDGE('',*,*,#3291,.T.);
#4229=ORIENTED_EDGE('',*,*,#3293,.T.);
#4230=ORIENTED_EDGE('',*,*,#3259,.T.);
#4231=ORIENTED_EDGE('',*,*,#3294,.F.);
#4232=ORIENTED_EDGE('',*,*,#3295,.T.);
#4233=ORIENTED_EDGE('',*,*,#3296,.F.);
#4234=ORIENTED_EDGE('',*,*,#3297,.T.);
#4235=ORIENTED_EDGE('',*,*,#3294,.T.);
#4236=ORIENTED_EDGE('',*,*,#3297,.F.);
#4237=ORIENTED_EDGE('',*,*,#3296,.T.);
#4238=ORIENTED_EDGE('',*,*,#3298,.F.);
#4239=ORIENTED_EDGE('',*,*,#3298,.T.);
#4240=ORIENTED_EDGE('',*,*,#3299,.T.);
#4241=ORIENTED_EDGE('',*,*,#3295,.F.);
#4242=ORIENTED_EDGE('',*,*,#3299,.F.);
#4243=ORIENTED_EDGE('',*,*,#3300,.F.);
#4244=ORIENTED_EDGE('',*,*,#3301,.T.);
#4245=ORIENTED_EDGE('',*,*,#3302,.F.);
#4246=ORIENTED_EDGE('',*,*,#3303,.T.);
#4247=ORIENTED_EDGE('',*,*,#3300,.T.);
#4248=ORIENTED_EDGE('',*,*,#3303,.F.);
#4249=ORIENTED_EDGE('',*,*,#3302,.T.);
#4250=ORIENTED_EDGE('',*,*,#3304,.F.);
#4251=ORIENTED_EDGE('',*,*,#3304,.T.);
#4252=ORIENTED_EDGE('',*,*,#3305,.T.);
#4253=ORIENTED_EDGE('',*,*,#3301,.F.);
#4254=ORIENTED_EDGE('',*,*,#3305,.F.);
#4255=ORIENTED_EDGE('',*,*,#3306,.F.);
#4256=ORIENTED_EDGE('',*,*,#3307,.T.);
#4257=ORIENTED_EDGE('',*,*,#3308,.T.);
#4258=ORIENTED_EDGE('',*,*,#3309,.T.);
#4259=ORIENTED_EDGE('',*,*,#3308,.F.);
#4260=ORIENTED_EDGE('',*,*,#3306,.T.);
#4261=ORIENTED_EDGE('',*,*,#3310,.T.);
#4262=ORIENTED_EDGE('',*,*,#3307,.F.);
#4263=ORIENTED_EDGE('',*,*,#3310,.F.);
#4264=ORIENTED_EDGE('',*,*,#3309,.F.);
#4265=ORIENTED_EDGE('',*,*,#3311,.T.);
#4266=ORIENTED_EDGE('',*,*,#3312,.T.);
#4267=ORIENTED_EDGE('',*,*,#3313,.T.);
#4268=ORIENTED_EDGE('',*,*,#3314,.T.);
#4269=ORIENTED_EDGE('',*,*,#3315,.T.);
#4270=ORIENTED_EDGE('',*,*,#3316,.T.);
#4271=ORIENTED_EDGE('',*,*,#3317,.T.);
#4272=ORIENTED_EDGE('',*,*,#3318,.T.);
#4273=ORIENTED_EDGE('',*,*,#3319,.F.);
#4274=ORIENTED_EDGE('',*,*,#3320,.T.);
#4275=ORIENTED_EDGE('',*,*,#3321,.F.);
#4276=ORIENTED_EDGE('',*,*,#3322,.F.);
#4277=ORIENTED_EDGE('',*,*,#3323,.F.);
#4278=ORIENTED_EDGE('',*,*,#3324,.F.);
#4279=ORIENTED_EDGE('',*,*,#3320,.F.);
#4280=ORIENTED_EDGE('',*,*,#3325,.F.);
#4281=ORIENTED_EDGE('',*,*,#3326,.T.);
#4282=ORIENTED_EDGE('',*,*,#3327,.F.);
#4283=ORIENTED_EDGE('',*,*,#3326,.F.);
#4284=ORIENTED_EDGE('',*,*,#3328,.F.);
#4285=ORIENTED_EDGE('',*,*,#3322,.T.);
#4286=ORIENTED_EDGE('',*,*,#3329,.F.);
#4287=ORIENTED_EDGE('',*,*,#3330,.T.);
#4288=ORIENTED_EDGE('',*,*,#3331,.F.);
#4289=ORIENTED_EDGE('',*,*,#3330,.F.);
#4290=ORIENTED_EDGE('',*,*,#3329,.T.);
#4291=ORIENTED_EDGE('',*,*,#3332,.F.);
#4292=ORIENTED_EDGE('',*,*,#3333,.F.);
#4293=ORIENTED_EDGE('',*,*,#3334,.T.);
#4294=ORIENTED_EDGE('',*,*,#3335,.F.);
#4295=ORIENTED_EDGE('',*,*,#3334,.F.);
#4296=ORIENTED_EDGE('',*,*,#3333,.T.);
#4297=ORIENTED_EDGE('',*,*,#3336,.F.);
#4298=ORIENTED_EDGE('',*,*,#3337,.F.);
#4299=ORIENTED_EDGE('',*,*,#3317,.F.);
#4300=ORIENTED_EDGE('',*,*,#3338,.F.);
#4301=ORIENTED_EDGE('',*,*,#3313,.F.);
#4302=ORIENTED_EDGE('',*,*,#3335,.T.);
#4303=ORIENTED_EDGE('',*,*,#3327,.T.);
#4304=ORIENTED_EDGE('',*,*,#3331,.T.);
#4305=ORIENTED_EDGE('',*,*,#3339,.F.);
#4306=ORIENTED_EDGE('',*,*,#3340,.T.);
#4307=ORIENTED_EDGE('',*,*,#3332,.T.);
#4308=ORIENTED_EDGE('',*,*,#3340,.F.);
#4309=ORIENTED_EDGE('',*,*,#3341,.F.);
#4310=ORIENTED_EDGE('',*,*,#3342,.T.);
#4311=ORIENTED_EDGE('',*,*,#3336,.T.);
#4312=ORIENTED_EDGE('',*,*,#3342,.F.);
#4313=ORIENTED_EDGE('',*,*,#3343,.F.);
#4314=ORIENTED_EDGE('',*,*,#3344,.T.);
#4315=ORIENTED_EDGE('',*,*,#3325,.T.);
#4316=ORIENTED_EDGE('',*,*,#3319,.T.);
#4317=ORIENTED_EDGE('',*,*,#3324,.T.);
#4318=ORIENTED_EDGE('',*,*,#3345,.T.);
#4319=ORIENTED_EDGE('',*,*,#3346,.F.);
#4320=ORIENTED_EDGE('',*,*,#3345,.F.);
#4321=ORIENTED_EDGE('',*,*,#3323,.T.);
#4322=ORIENTED_EDGE('',*,*,#3328,.T.);
#4323=ORIENTED_EDGE('',*,*,#3321,.T.);
#4324=ORIENTED_EDGE('',*,*,#3344,.F.);
#4325=ORIENTED_EDGE('',*,*,#3347,.F.);
#4326=ORIENTED_EDGE('',*,*,#3314,.F.);
#4327=ORIENTED_EDGE('',*,*,#3338,.T.);
#4328=ORIENTED_EDGE('',*,*,#3316,.F.);
#4329=ORIENTED_EDGE('',*,*,#3346,.T.);
#4330=ORIENTED_EDGE('',*,*,#3348,.T.);
#4331=ORIENTED_EDGE('',*,*,#3318,.F.);
#4332=ORIENTED_EDGE('',*,*,#3337,.T.);
#4333=ORIENTED_EDGE('',*,*,#3312,.F.);
#4334=ORIENTED_EDGE('',*,*,#3343,.T.);
#4335=ORIENTED_EDGE('',*,*,#3348,.F.);
#4336=ORIENTED_EDGE('',*,*,#3311,.F.);
#4337=ORIENTED_EDGE('',*,*,#3347,.T.);
#4338=ORIENTED_EDGE('',*,*,#3315,.F.);
#4339=ORIENTED_EDGE('',*,*,#3339,.T.);
#4340=ORIENTED_EDGE('',*,*,#3341,.T.);
#4341=ORIENTED_EDGE('',*,*,#3349,.F.);
#4342=ORIENTED_EDGE('',*,*,#3350,.T.);
#4343=ORIENTED_EDGE('',*,*,#3351,.T.);
#4344=ORIENTED_EDGE('',*,*,#3352,.F.);
#4345=ORIENTED_EDGE('',*,*,#3353,.F.);
#4346=ORIENTED_EDGE('',*,*,#3354,.T.);
#4347=ORIENTED_EDGE('',*,*,#3355,.T.);
#4348=ORIENTED_EDGE('',*,*,#3350,.F.);
#4349=ORIENTED_EDGE('',*,*,#3356,.F.);
#4350=ORIENTED_EDGE('',*,*,#3357,.T.);
#4351=ORIENTED_EDGE('',*,*,#3358,.T.);
#4352=ORIENTED_EDGE('',*,*,#3354,.F.);
#4353=ORIENTED_EDGE('',*,*,#3359,.F.);
#4354=ORIENTED_EDGE('',*,*,#3360,.T.);
#4355=ORIENTED_EDGE('',*,*,#3361,.T.);
#4356=ORIENTED_EDGE('',*,*,#3357,.F.);
#4357=ORIENTED_EDGE('',*,*,#3362,.F.);
#4358=ORIENTED_EDGE('',*,*,#3363,.T.);
#4359=ORIENTED_EDGE('',*,*,#3364,.T.);
#4360=ORIENTED_EDGE('',*,*,#3360,.F.);
#4361=ORIENTED_EDGE('',*,*,#3365,.F.);
#4362=ORIENTED_EDGE('',*,*,#3352,.T.);
#4363=ORIENTED_EDGE('',*,*,#3366,.T.);
#4364=ORIENTED_EDGE('',*,*,#3363,.F.);
#4365=ORIENTED_EDGE('',*,*,#3366,.F.);
#4366=ORIENTED_EDGE('',*,*,#3351,.F.);
#4367=ORIENTED_EDGE('',*,*,#3355,.F.);
#4368=ORIENTED_EDGE('',*,*,#3358,.F.);
#4369=ORIENTED_EDGE('',*,*,#3361,.F.);
#4370=ORIENTED_EDGE('',*,*,#3364,.F.);
#4371=ORIENTED_EDGE('',*,*,#3367,.F.);
#4372=ORIENTED_EDGE('',*,*,#3349,.T.);
#4373=ORIENTED_EDGE('',*,*,#3365,.T.);
#4374=ORIENTED_EDGE('',*,*,#3362,.T.);
#4375=ORIENTED_EDGE('',*,*,#3359,.T.);
#4376=ORIENTED_EDGE('',*,*,#3356,.T.);
#4377=ORIENTED_EDGE('',*,*,#3353,.T.);
#4378=ORIENTED_EDGE('',*,*,#3368,.F.);
#4379=ORIENTED_EDGE('',*,*,#3369,.T.);
#4380=ORIENTED_EDGE('',*,*,#3367,.T.);
#4381=ORIENTED_EDGE('',*,*,#3369,.F.);
#4382=ORIENTED_EDGE('',*,*,#3370,.F.);
#4383=ORIENTED_EDGE('',*,*,#3371,.T.);
#4384=ORIENTED_EDGE('',*,*,#3368,.T.);
#4385=ORIENTED_EDGE('',*,*,#3371,.F.);
#4386=ORIENTED_EDGE('',*,*,#3372,.F.);
#4387=ORIENTED_EDGE('',*,*,#3373,.T.);
#4388=ORIENTED_EDGE('',*,*,#3370,.T.);
#4389=ORIENTED_EDGE('',*,*,#3373,.F.);
#4390=ORIENTED_EDGE('',*,*,#3372,.T.);
#4391=ORIENTED_EDGE('',*,*,#3374,.F.);
#4392=ORIENTED_EDGE('',*,*,#3375,.T.);
#4393=ORIENTED_EDGE('',*,*,#3376,.F.);
#4394=ORIENTED_EDGE('',*,*,#3375,.F.);
#4395=ORIENTED_EDGE('',*,*,#3377,.F.);
#4396=ORIENTED_EDGE('',*,*,#3378,.T.);
#4397=ORIENTED_EDGE('',*,*,#3379,.F.);
#4398=ORIENTED_EDGE('',*,*,#3378,.F.);
#4399=ORIENTED_EDGE('',*,*,#3380,.F.);
#4400=ORIENTED_EDGE('',*,*,#3381,.T.);
#4401=ORIENTED_EDGE('',*,*,#3382,.F.);
#4402=ORIENTED_EDGE('',*,*,#3381,.F.);
#4403=ORIENTED_EDGE('',*,*,#3383,.F.);
#4404=ORIENTED_EDGE('',*,*,#3384,.T.);
#4405=ORIENTED_EDGE('',*,*,#3385,.F.);
#4406=ORIENTED_EDGE('',*,*,#3386,.F.);
#4407=ORIENTED_EDGE('',*,*,#3383,.T.);
#4408=ORIENTED_EDGE('',*,*,#3387,.F.);
#4409=ORIENTED_EDGE('',*,*,#3388,.F.);
#4410=ORIENTED_EDGE('',*,*,#3389,.F.);
#4411=ORIENTED_EDGE('',*,*,#3386,.T.);
#4412=ORIENTED_EDGE('',*,*,#3390,.T.);
#4413=ORIENTED_EDGE('',*,*,#3391,.T.);
#4414=ORIENTED_EDGE('',*,*,#3392,.T.);
#4415=ORIENTED_EDGE('',*,*,#3393,.T.);
#4416=ORIENTED_EDGE('',*,*,#3394,.T.);
#4417=ORIENTED_EDGE('',*,*,#3395,.T.);
#4418=ORIENTED_EDGE('',*,*,#3396,.T.);
#4419=ORIENTED_EDGE('',*,*,#3397,.T.);
#4420=ORIENTED_EDGE('',*,*,#3398,.T.);
#4421=ORIENTED_EDGE('',*,*,#3399,.T.);
#4422=ORIENTED_EDGE('',*,*,#3387,.T.);
#4423=ORIENTED_EDGE('',*,*,#3376,.T.);
#4424=ORIENTED_EDGE('',*,*,#3379,.T.);
#4425=ORIENTED_EDGE('',*,*,#3382,.T.);
#4426=ORIENTED_EDGE('',*,*,#3385,.T.);
#4427=ORIENTED_EDGE('',*,*,#3400,.F.);
#4428=ORIENTED_EDGE('',*,*,#3401,.F.);
#4429=ORIENTED_EDGE('',*,*,#3390,.F.);
#4430=ORIENTED_EDGE('',*,*,#3388,.T.);
#4431=ORIENTED_EDGE('',*,*,#3399,.F.);
#4432=ORIENTED_EDGE('',*,*,#3402,.T.);
#4433=ORIENTED_EDGE('',*,*,#3403,.T.);
#4434=ORIENTED_EDGE('',*,*,#3401,.T.);
#4435=ORIENTED_EDGE('',*,*,#3404,.T.);
#4436=ORIENTED_EDGE('',*,*,#3405,.T.);
#4437=ORIENTED_EDGE('',*,*,#3391,.F.);
#4438=ORIENTED_EDGE('',*,*,#3406,.F.);
#4439=ORIENTED_EDGE('',*,*,#3393,.F.);
#4440=ORIENTED_EDGE('',*,*,#3407,.F.);
#4441=ORIENTED_EDGE('',*,*,#3408,.T.);
#4442=ORIENTED_EDGE('',*,*,#3406,.T.);
#4443=ORIENTED_EDGE('',*,*,#3409,.F.);
#4444=ORIENTED_EDGE('',*,*,#3410,.F.);
#4445=ORIENTED_EDGE('',*,*,#3394,.F.);
#4446=ORIENTED_EDGE('',*,*,#3389,.T.);
#4447=ORIENTED_EDGE('',*,*,#3403,.F.);
#4448=ORIENTED_EDGE('',*,*,#3411,.T.);
#4449=ORIENTED_EDGE('',*,*,#3412,.F.);
#4450=ORIENTED_EDGE('',*,*,#3413,.T.);
#4451=ORIENTED_EDGE('',*,*,#3414,.F.);
#4452=ORIENTED_EDGE('',*,*,#3409,.T.);
#4453=ORIENTED_EDGE('',*,*,#3408,.F.);
#4454=ORIENTED_EDGE('',*,*,#3415,.T.);
#4455=ORIENTED_EDGE('',*,*,#3404,.F.);
#4456=ORIENTED_EDGE('',*,*,#3400,.T.);
#4457=ORIENTED_EDGE('',*,*,#3384,.F.);
#4458=ORIENTED_EDGE('',*,*,#3374,.T.);
#4459=ORIENTED_EDGE('',*,*,#3377,.T.);
#4460=ORIENTED_EDGE('',*,*,#3380,.T.);
#4461=ORIENTED_EDGE('',*,*,#3416,.T.);
#4462=ORIENTED_EDGE('',*,*,#3407,.T.);
#4463=ORIENTED_EDGE('',*,*,#3392,.F.);
#4464=ORIENTED_EDGE('',*,*,#3405,.F.);
#4465=ORIENTED_EDGE('',*,*,#3415,.F.);
#4466=ORIENTED_EDGE('',*,*,#3417,.F.);
#4467=ORIENTED_EDGE('',*,*,#3412,.T.);
#4468=ORIENTED_EDGE('',*,*,#3418,.F.);
#4469=ORIENTED_EDGE('',*,*,#3397,.F.);
#4470=ORIENTED_EDGE('',*,*,#3417,.T.);
#4471=ORIENTED_EDGE('',*,*,#3396,.F.);
#4472=ORIENTED_EDGE('',*,*,#3419,.F.);
#4473=ORIENTED_EDGE('',*,*,#3413,.F.);
#4474=ORIENTED_EDGE('',*,*,#3418,.T.);
#4475=ORIENTED_EDGE('',*,*,#3411,.F.);
#4476=ORIENTED_EDGE('',*,*,#3402,.F.);
#4477=ORIENTED_EDGE('',*,*,#3398,.F.);
#4478=ORIENTED_EDGE('',*,*,#3410,.T.);
#4479=ORIENTED_EDGE('',*,*,#3414,.T.);
#4480=ORIENTED_EDGE('',*,*,#3419,.T.);
#4481=ORIENTED_EDGE('',*,*,#3395,.F.);
#4482=ORIENTED_EDGE('',*,*,#3420,.F.);
#4483=ORIENTED_EDGE('',*,*,#3421,.F.);
#4484=ORIENTED_EDGE('',*,*,#3416,.F.);
#4485=ORIENTED_EDGE('',*,*,#3422,.T.);
#4486=ORIENTED_EDGE('',*,*,#3420,.T.);
#4487=ORIENTED_EDGE('',*,*,#3422,.F.);
#4488=ORIENTED_EDGE('',*,*,#3421,.T.);
#4489=ORIENTED_EDGE('',*,*,#3423,.T.);
#4490=ORIENTED_EDGE('',*,*,#3424,.T.);
#4491=ORIENTED_EDGE('',*,*,#3423,.F.);
#4492=ORIENTED_EDGE('',*,*,#3424,.F.);
#4493=ORIENTED_EDGE('',*,*,#3425,.F.);
#4494=ORIENTED_EDGE('',*,*,#3426,.T.);
#4495=ORIENTED_EDGE('',*,*,#3427,.T.);
#4496=ORIENTED_EDGE('',*,*,#3426,.F.);
#4497=ORIENTED_EDGE('',*,*,#3427,.F.);
#4498=ORIENTED_EDGE('',*,*,#3428,.F.);
#4499=ORIENTED_EDGE('',*,*,#3429,.T.);
#4500=ORIENTED_EDGE('',*,*,#3430,.T.);
#4501=ORIENTED_EDGE('',*,*,#3429,.F.);
#4502=ORIENTED_EDGE('',*,*,#3428,.T.);
#4503=ORIENTED_EDGE('',*,*,#3430,.F.);
#4504=ORIENTED_EDGE('',*,*,#3425,.T.);
#4505=ORIENTED_EDGE('',*,*,#3431,.F.);
#4506=ORIENTED_EDGE('',*,*,#3432,.T.);
#4507=ORIENTED_EDGE('',*,*,#3433,.T.);
#4508=ORIENTED_EDGE('',*,*,#3432,.F.);
#4509=ORIENTED_EDGE('',*,*,#3434,.F.);
#4510=ORIENTED_EDGE('',*,*,#3435,.T.);
#4511=ORIENTED_EDGE('',*,*,#3436,.T.);
#4512=ORIENTED_EDGE('',*,*,#3435,.F.);
#4513=ORIENTED_EDGE('',*,*,#3434,.T.);
#4514=ORIENTED_EDGE('',*,*,#3431,.T.);
#4515=ORIENTED_EDGE('',*,*,#3436,.F.);
#4516=ORIENTED_EDGE('',*,*,#3433,.F.);
#4517=ORIENTED_EDGE('',*,*,#3437,.F.);
#4518=ORIENTED_EDGE('',*,*,#3438,.T.);
#4519=ORIENTED_EDGE('',*,*,#3439,.F.);
#4520=ORIENTED_EDGE('',*,*,#3440,.F.);
#4521=ORIENTED_EDGE('',*,*,#3441,.F.);
#4522=ORIENTED_EDGE('',*,*,#3442,.T.);
#4523=ORIENTED_EDGE('',*,*,#3443,.F.);
#4524=ORIENTED_EDGE('',*,*,#3444,.F.);
#4525=ORIENTED_EDGE('',*,*,#3442,.F.);
#4526=ORIENTED_EDGE('',*,*,#3445,.F.);
#4527=ORIENTED_EDGE('',*,*,#3438,.F.);
#4528=ORIENTED_EDGE('',*,*,#3446,.F.);
#4529=ORIENTED_EDGE('',*,*,#3440,.T.);
#4530=ORIENTED_EDGE('',*,*,#3447,.F.);
#4531=ORIENTED_EDGE('',*,*,#3448,.T.);
#4532=ORIENTED_EDGE('',*,*,#3449,.T.);
#4533=ORIENTED_EDGE('',*,*,#3448,.F.);
#4534=ORIENTED_EDGE('',*,*,#3445,.T.);
#4535=ORIENTED_EDGE('',*,*,#3441,.T.);
#4536=ORIENTED_EDGE('',*,*,#3446,.T.);
#4537=ORIENTED_EDGE('',*,*,#3439,.T.);
#4538=ORIENTED_EDGE('',*,*,#3437,.T.);
#4539=ORIENTED_EDGE('',*,*,#3450,.F.);
#4540=ORIENTED_EDGE('',*,*,#3451,.T.);
#4541=ORIENTED_EDGE('',*,*,#3452,.T.);
#4542=ORIENTED_EDGE('',*,*,#3451,.F.);
#4543=ORIENTED_EDGE('',*,*,#3443,.T.);
#4544=ORIENTED_EDGE('',*,*,#3444,.T.);
#4545=ORIENTED_EDGE('',*,*,#3450,.T.);
#4546=ORIENTED_EDGE('',*,*,#3447,.T.);
#4547=ORIENTED_EDGE('',*,*,#3452,.F.);
#4548=ORIENTED_EDGE('',*,*,#3449,.F.);
#4549=ORIENTED_EDGE('',*,*,#3453,.F.);
#4550=ORIENTED_EDGE('',*,*,#3454,.F.);
#4551=ORIENTED_EDGE('',*,*,#3455,.T.);
#4552=ORIENTED_EDGE('',*,*,#3453,.T.);
#4553=ORIENTED_EDGE('',*,*,#3455,.F.);
#4554=ORIENTED_EDGE('',*,*,#3456,.F.);
#4555=ORIENTED_EDGE('',*,*,#3457,.T.);
#4556=ORIENTED_EDGE('',*,*,#3454,.T.);
#4557=ORIENTED_EDGE('',*,*,#3457,.F.);
#4558=ORIENTED_EDGE('',*,*,#3458,.F.);
#4559=ORIENTED_EDGE('',*,*,#3459,.T.);
#4560=ORIENTED_EDGE('',*,*,#3456,.T.);
#4561=ORIENTED_EDGE('',*,*,#3459,.F.);
#4562=ORIENTED_EDGE('',*,*,#3458,.T.);
#4563=ORIENTED_EDGE('',*,*,#3460,.F.);
#4564=ORIENTED_EDGE('',*,*,#3461,.F.);
#4565=ORIENTED_EDGE('',*,*,#3462,.T.);
#4566=ORIENTED_EDGE('',*,*,#3460,.T.);
#4567=ORIENTED_EDGE('',*,*,#3462,.F.);
#4568=ORIENTED_EDGE('',*,*,#3463,.F.);
#4569=ORIENTED_EDGE('',*,*,#3464,.T.);
#4570=ORIENTED_EDGE('',*,*,#3461,.T.);
#4571=ORIENTED_EDGE('',*,*,#3464,.F.);
#4572=ORIENTED_EDGE('',*,*,#3465,.F.);
#4573=ORIENTED_EDGE('',*,*,#3466,.T.);
#4574=ORIENTED_EDGE('',*,*,#3463,.T.);
#4575=ORIENTED_EDGE('',*,*,#3466,.F.);
#4576=ORIENTED_EDGE('',*,*,#3465,.T.);
#4577=ORIENTED_EDGE('',*,*,#3467,.T.);
#4578=ORIENTED_EDGE('',*,*,#3468,.T.);
#4579=ORIENTED_EDGE('',*,*,#3469,.T.);
#4580=ORIENTED_EDGE('',*,*,#3470,.F.);
#4581=ORIENTED_EDGE('',*,*,#3471,.T.);
#4582=ORIENTED_EDGE('',*,*,#3472,.T.);
#4583=ORIENTED_EDGE('',*,*,#3473,.T.);
#4584=ORIENTED_EDGE('',*,*,#3468,.F.);
#4585=ORIENTED_EDGE('',*,*,#3474,.T.);
#4586=ORIENTED_EDGE('',*,*,#3475,.T.);
#4587=ORIENTED_EDGE('',*,*,#3476,.T.);
#4588=ORIENTED_EDGE('',*,*,#3472,.F.);
#4589=ORIENTED_EDGE('',*,*,#3477,.T.);
#4590=ORIENTED_EDGE('',*,*,#3478,.T.);
#4591=ORIENTED_EDGE('',*,*,#3479,.T.);
#4592=ORIENTED_EDGE('',*,*,#3475,.F.);
#4593=ORIENTED_EDGE('',*,*,#3480,.T.);
#4594=ORIENTED_EDGE('',*,*,#3481,.T.);
#4595=ORIENTED_EDGE('',*,*,#3482,.T.);
#4596=ORIENTED_EDGE('',*,*,#3478,.F.);
#4597=ORIENTED_EDGE('',*,*,#3483,.T.);
#4598=ORIENTED_EDGE('',*,*,#3470,.T.);
#4599=ORIENTED_EDGE('',*,*,#3484,.T.);
#4600=ORIENTED_EDGE('',*,*,#3481,.F.);
#4601=ORIENTED_EDGE('',*,*,#3483,.F.);
#4602=ORIENTED_EDGE('',*,*,#3480,.F.);
#4603=ORIENTED_EDGE('',*,*,#3477,.F.);
#4604=ORIENTED_EDGE('',*,*,#3474,.F.);
#4605=ORIENTED_EDGE('',*,*,#3471,.F.);
#4606=ORIENTED_EDGE('',*,*,#3467,.F.);
#4607=ORIENTED_EDGE('',*,*,#3484,.F.);
#4608=ORIENTED_EDGE('',*,*,#3469,.F.);
#4609=ORIENTED_EDGE('',*,*,#3473,.F.);
#4610=ORIENTED_EDGE('',*,*,#3476,.F.);
#4611=ORIENTED_EDGE('',*,*,#3479,.F.);
#4612=ORIENTED_EDGE('',*,*,#3482,.F.);
#4613=ORIENTED_EDGE('',*,*,#3485,.F.);
#4614=ORIENTED_EDGE('',*,*,#3486,.F.);
#4615=ORIENTED_EDGE('',*,*,#3487,.T.);
#4616=ORIENTED_EDGE('',*,*,#3488,.T.);
#4617=ORIENTED_EDGE('',*,*,#3489,.F.);
#4618=ORIENTED_EDGE('',*,*,#3490,.F.);
#4619=ORIENTED_EDGE('',*,*,#3491,.T.);
#4620=ORIENTED_EDGE('',*,*,#3492,.T.);
#4621=ORIENTED_EDGE('',*,*,#3487,.F.);
#4622=ORIENTED_EDGE('',*,*,#3493,.F.);
#4623=ORIENTED_EDGE('',*,*,#3494,.T.);
#4624=ORIENTED_EDGE('',*,*,#3495,.T.);
#4625=ORIENTED_EDGE('',*,*,#3491,.F.);
#4626=ORIENTED_EDGE('',*,*,#3496,.F.);
#4627=ORIENTED_EDGE('',*,*,#3497,.T.);
#4628=ORIENTED_EDGE('',*,*,#3498,.T.);
#4629=ORIENTED_EDGE('',*,*,#3494,.F.);
#4630=ORIENTED_EDGE('',*,*,#3499,.F.);
#4631=ORIENTED_EDGE('',*,*,#3500,.T.);
#4632=ORIENTED_EDGE('',*,*,#3501,.T.);
#4633=ORIENTED_EDGE('',*,*,#3497,.F.);
#4634=ORIENTED_EDGE('',*,*,#3502,.F.);
#4635=ORIENTED_EDGE('',*,*,#3489,.T.);
#4636=ORIENTED_EDGE('',*,*,#3503,.T.);
#4637=ORIENTED_EDGE('',*,*,#3500,.F.);
#4638=ORIENTED_EDGE('',*,*,#3503,.F.);
#4639=ORIENTED_EDGE('',*,*,#3488,.F.);
#4640=ORIENTED_EDGE('',*,*,#3492,.F.);
#4641=ORIENTED_EDGE('',*,*,#3495,.F.);
#4642=ORIENTED_EDGE('',*,*,#3498,.F.);
#4643=ORIENTED_EDGE('',*,*,#3501,.F.);
#4644=ORIENTED_EDGE('',*,*,#3504,.F.);
#4645=ORIENTED_EDGE('',*,*,#3486,.T.);
#4646=ORIENTED_EDGE('',*,*,#3502,.T.);
#4647=ORIENTED_EDGE('',*,*,#3499,.T.);
#4648=ORIENTED_EDGE('',*,*,#3496,.T.);
#4649=ORIENTED_EDGE('',*,*,#3493,.T.);
#4650=ORIENTED_EDGE('',*,*,#3490,.T.);
#4651=ORIENTED_EDGE('',*,*,#3505,.F.);
#4652=ORIENTED_EDGE('',*,*,#3506,.T.);
#4653=ORIENTED_EDGE('',*,*,#3504,.T.);
#4654=ORIENTED_EDGE('',*,*,#3506,.F.);
#4655=ORIENTED_EDGE('',*,*,#3485,.T.);
#4656=ORIENTED_EDGE('',*,*,#3507,.T.);
#4657=ORIENTED_EDGE('',*,*,#3505,.T.);
#4658=ORIENTED_EDGE('',*,*,#3507,.F.);
#4659=ORIENTED_EDGE('',*,*,#3508,.F.);
#4660=ORIENTED_EDGE('',*,*,#3509,.T.);
#4661=ORIENTED_EDGE('',*,*,#3510,.F.);
#4662=ORIENTED_EDGE('',*,*,#3509,.F.);
#4663=ORIENTED_EDGE('',*,*,#3508,.T.);
#4664=ORIENTED_EDGE('',*,*,#3511,.T.);
#4665=ORIENTED_EDGE('',*,*,#3512,.F.);
#4666=ORIENTED_EDGE('',*,*,#3513,.F.);
#4667=ORIENTED_EDGE('',*,*,#3514,.F.);
#4668=ORIENTED_EDGE('',*,*,#3511,.F.);
#4669=ORIENTED_EDGE('',*,*,#3515,.T.);
#4670=ORIENTED_EDGE('',*,*,#3513,.T.);
#4671=ORIENTED_EDGE('',*,*,#3515,.F.);
#4672=ORIENTED_EDGE('',*,*,#3514,.T.);
#4673=ORIENTED_EDGE('',*,*,#3516,.T.);
#4674=ORIENTED_EDGE('',*,*,#3517,.T.);
#4675=ORIENTED_EDGE('',*,*,#3516,.F.);
#4676=ORIENTED_EDGE('',*,*,#3518,.F.);
#4677=ORIENTED_EDGE('',*,*,#3519,.T.);
#4678=ORIENTED_EDGE('',*,*,#3512,.T.);
#4679=ORIENTED_EDGE('',*,*,#3519,.F.);
#4680=ORIENTED_EDGE('',*,*,#3518,.T.);
#4681=ORIENTED_EDGE('',*,*,#3510,.T.);
#4682=ORIENTED_EDGE('',*,*,#3517,.F.);
#4683=ORIENTED_EDGE('',*,*,#3520,.F.);
#4684=ORIENTED_EDGE('',*,*,#3521,.T.);
#4685=ORIENTED_EDGE('',*,*,#3522,.T.);
#4686=ORIENTED_EDGE('',*,*,#3521,.F.);
#4687=ORIENTED_EDGE('',*,*,#3523,.F.);
#4688=ORIENTED_EDGE('',*,*,#3524,.T.);
#4689=ORIENTED_EDGE('',*,*,#3525,.T.);
#4690=ORIENTED_EDGE('',*,*,#3524,.F.);
#4691=ORIENTED_EDGE('',*,*,#3523,.T.);
#4692=ORIENTED_EDGE('',*,*,#3520,.T.);
#4693=ORIENTED_EDGE('',*,*,#3525,.F.);
#4694=ORIENTED_EDGE('',*,*,#3522,.F.);
#4695=ORIENTED_EDGE('',*,*,#3526,.F.);
#4696=ORIENTED_EDGE('',*,*,#3527,.T.);
#4697=ORIENTED_EDGE('',*,*,#3528,.F.);
#4698=ORIENTED_EDGE('',*,*,#3527,.F.);
#4699=ORIENTED_EDGE('',*,*,#3529,.F.);
#4700=ORIENTED_EDGE('',*,*,#3530,.T.);
#4701=ORIENTED_EDGE('',*,*,#3531,.F.);
#4702=ORIENTED_EDGE('',*,*,#3530,.F.);
#4703=ORIENTED_EDGE('',*,*,#3532,.F.);
#4704=ORIENTED_EDGE('',*,*,#3533,.F.);
#4705=ORIENTED_EDGE('',*,*,#3534,.F.);
#4706=ORIENTED_EDGE('',*,*,#3535,.T.);
#4707=ORIENTED_EDGE('',*,*,#3532,.T.);
#4708=ORIENTED_EDGE('',*,*,#3536,.F.);
#4709=ORIENTED_EDGE('',*,*,#3537,.F.);
#4710=ORIENTED_EDGE('',*,*,#3538,.F.);
#4711=ORIENTED_EDGE('',*,*,#3535,.F.);
#4712=ORIENTED_EDGE('',*,*,#3539,.T.);
#4713=ORIENTED_EDGE('',*,*,#3540,.F.);
#4714=ORIENTED_EDGE('',*,*,#3536,.T.);
#4715=ORIENTED_EDGE('',*,*,#3526,.T.);
#4716=ORIENTED_EDGE('',*,*,#3529,.T.);
#4717=ORIENTED_EDGE('',*,*,#3534,.T.);
#4718=ORIENTED_EDGE('',*,*,#3541,.F.);
#4719=ORIENTED_EDGE('',*,*,#3542,.F.);
#4720=ORIENTED_EDGE('',*,*,#3539,.F.);
#4721=ORIENTED_EDGE('',*,*,#3537,.T.);
#4722=ORIENTED_EDGE('',*,*,#3540,.T.);
#4723=ORIENTED_EDGE('',*,*,#3542,.T.);
#4724=ORIENTED_EDGE('',*,*,#3543,.F.);
#4725=ORIENTED_EDGE('',*,*,#3538,.T.);
#4726=ORIENTED_EDGE('',*,*,#3543,.T.);
#4727=ORIENTED_EDGE('',*,*,#3541,.T.);
#4728=ORIENTED_EDGE('',*,*,#3533,.T.);
#4729=ORIENTED_EDGE('',*,*,#3528,.T.);
#4730=ORIENTED_EDGE('',*,*,#3531,.T.);
#4731=ORIENTED_EDGE('',*,*,#3544,.F.);
#4732=ORIENTED_EDGE('',*,*,#3545,.T.);
#4733=ORIENTED_EDGE('',*,*,#3546,.T.);
#4734=ORIENTED_EDGE('',*,*,#3545,.F.);
#4735=ORIENTED_EDGE('',*,*,#3547,.F.);
#4736=ORIENTED_EDGE('',*,*,#3548,.T.);
#4737=ORIENTED_EDGE('',*,*,#3549,.T.);
#4738=ORIENTED_EDGE('',*,*,#3548,.F.);
#4739=ORIENTED_EDGE('',*,*,#3547,.T.);
#4740=ORIENTED_EDGE('',*,*,#3544,.T.);
#4741=ORIENTED_EDGE('',*,*,#3549,.F.);
#4742=ORIENTED_EDGE('',*,*,#3546,.F.);
#4743=ORIENTED_EDGE('',*,*,#3550,.F.);
#4744=ORIENTED_EDGE('',*,*,#3551,.T.);
#4745=ORIENTED_EDGE('',*,*,#3552,.F.);
#4746=ORIENTED_EDGE('',*,*,#3551,.F.);
#4747=ORIENTED_EDGE('',*,*,#3550,.T.);
#4748=ORIENTED_EDGE('',*,*,#3553,.T.);
#4749=ORIENTED_EDGE('',*,*,#3554,.F.);
#4750=ORIENTED_EDGE('',*,*,#3555,.F.);
#4751=ORIENTED_EDGE('',*,*,#3556,.F.);
#4752=ORIENTED_EDGE('',*,*,#3553,.F.);
#4753=ORIENTED_EDGE('',*,*,#3557,.T.);
#4754=ORIENTED_EDGE('',*,*,#3555,.T.);
#4755=ORIENTED_EDGE('',*,*,#3557,.F.);
#4756=ORIENTED_EDGE('',*,*,#3556,.T.);
#4757=ORIENTED_EDGE('',*,*,#3558,.T.);
#4758=ORIENTED_EDGE('',*,*,#3559,.T.);
#4759=ORIENTED_EDGE('',*,*,#3558,.F.);
#4760=ORIENTED_EDGE('',*,*,#3560,.F.);
#4761=ORIENTED_EDGE('',*,*,#3561,.T.);
#4762=ORIENTED_EDGE('',*,*,#3554,.T.);
#4763=ORIENTED_EDGE('',*,*,#3561,.F.);
#4764=ORIENTED_EDGE('',*,*,#3560,.T.);
#4765=ORIENTED_EDGE('',*,*,#3552,.T.);
#4766=ORIENTED_EDGE('',*,*,#3559,.F.);
#4767=ORIENTED_EDGE('',*,*,#3562,.F.);
#4768=ORIENTED_EDGE('',*,*,#3563,.T.);
#4769=ORIENTED_EDGE('',*,*,#3564,.T.);
#4770=ORIENTED_EDGE('',*,*,#3563,.F.);
#4771=ORIENTED_EDGE('',*,*,#3565,.F.);
#4772=ORIENTED_EDGE('',*,*,#3566,.T.);
#4773=ORIENTED_EDGE('',*,*,#3567,.T.);
#4774=ORIENTED_EDGE('',*,*,#3566,.F.);
#4775=ORIENTED_EDGE('',*,*,#3565,.T.);
#4776=ORIENTED_EDGE('',*,*,#3562,.T.);
#4777=ORIENTED_EDGE('',*,*,#3567,.F.);
#4778=ORIENTED_EDGE('',*,*,#3564,.F.);
#4779=ORIENTED_EDGE('',*,*,#3568,.F.);
#4780=ORIENTED_EDGE('',*,*,#3569,.T.);
#4781=ORIENTED_EDGE('',*,*,#3570,.F.);
#4782=ORIENTED_EDGE('',*,*,#3569,.F.);
#4783=ORIENTED_EDGE('',*,*,#3568,.T.);
#4784=ORIENTED_EDGE('',*,*,#3571,.F.);
#4785=ORIENTED_EDGE('',*,*,#3572,.T.);
#4786=ORIENTED_EDGE('',*,*,#3573,.F.);
#4787=ORIENTED_EDGE('',*,*,#3572,.F.);
#4788=ORIENTED_EDGE('',*,*,#3574,.F.);
#4789=ORIENTED_EDGE('',*,*,#3575,.T.);
#4790=ORIENTED_EDGE('',*,*,#3576,.F.);
#4791=ORIENTED_EDGE('',*,*,#3575,.F.);
#4792=ORIENTED_EDGE('',*,*,#3577,.F.);
#4793=ORIENTED_EDGE('',*,*,#3578,.T.);
#4794=ORIENTED_EDGE('',*,*,#3579,.F.);
#4795=ORIENTED_EDGE('',*,*,#3578,.F.);
#4796=ORIENTED_EDGE('',*,*,#3580,.F.);
#4797=ORIENTED_EDGE('',*,*,#3581,.T.);
#4798=ORIENTED_EDGE('',*,*,#3582,.F.);
#4799=ORIENTED_EDGE('',*,*,#3581,.F.);
#4800=ORIENTED_EDGE('',*,*,#3583,.F.);
#4801=ORIENTED_EDGE('',*,*,#3584,.T.);
#4802=ORIENTED_EDGE('',*,*,#3585,.F.);
#4803=ORIENTED_EDGE('',*,*,#3584,.F.);
#4804=ORIENTED_EDGE('',*,*,#3586,.T.);
#4805=ORIENTED_EDGE('',*,*,#3587,.T.);
#4806=ORIENTED_EDGE('',*,*,#3588,.F.);
#4807=ORIENTED_EDGE('',*,*,#3589,.F.);
#4808=ORIENTED_EDGE('',*,*,#3590,.T.);
#4809=ORIENTED_EDGE('',*,*,#3589,.T.);
#4810=ORIENTED_EDGE('',*,*,#3591,.F.);
#4811=ORIENTED_EDGE('',*,*,#3592,.F.);
#4812=ORIENTED_EDGE('',*,*,#3585,.T.);
#4813=ORIENTED_EDGE('',*,*,#3582,.T.);
#4814=ORIENTED_EDGE('',*,*,#3579,.T.);
#4815=ORIENTED_EDGE('',*,*,#3576,.T.);
#4816=ORIENTED_EDGE('',*,*,#3573,.T.);
#4817=ORIENTED_EDGE('',*,*,#3593,.T.);
#4818=ORIENTED_EDGE('',*,*,#3592,.T.);
#4819=ORIENTED_EDGE('',*,*,#3594,.F.);
#4820=ORIENTED_EDGE('',*,*,#3595,.F.);
#4821=ORIENTED_EDGE('',*,*,#3596,.T.);
#4822=ORIENTED_EDGE('',*,*,#3595,.T.);
#4823=ORIENTED_EDGE('',*,*,#3597,.F.);
#4824=ORIENTED_EDGE('',*,*,#3587,.F.);
#4825=ORIENTED_EDGE('',*,*,#3583,.T.);
#4826=ORIENTED_EDGE('',*,*,#3580,.T.);
#4827=ORIENTED_EDGE('',*,*,#3577,.T.);
#4828=ORIENTED_EDGE('',*,*,#3574,.T.);
#4829=ORIENTED_EDGE('',*,*,#3571,.T.);
#4830=ORIENTED_EDGE('',*,*,#3597,.T.);
#4831=ORIENTED_EDGE('',*,*,#3594,.T.);
#4832=ORIENTED_EDGE('',*,*,#3591,.T.);
#4833=ORIENTED_EDGE('',*,*,#3588,.T.);
#4834=ORIENTED_EDGE('',*,*,#3570,.T.);
#4835=ORIENTED_EDGE('',*,*,#3596,.F.);
#4836=ORIENTED_EDGE('',*,*,#3586,.F.);
#4837=ORIENTED_EDGE('',*,*,#3590,.F.);
#4838=ORIENTED_EDGE('',*,*,#3593,.F.);
#4839=ORIENTED_EDGE('',*,*,#3598,.F.);
#4840=ORIENTED_EDGE('',*,*,#3599,.F.);
#4841=ORIENTED_EDGE('',*,*,#3600,.F.);
#4842=ORIENTED_EDGE('',*,*,#3601,.F.);
#4843=ORIENTED_EDGE('',*,*,#3602,.F.);
#4844=ORIENTED_EDGE('',*,*,#3601,.T.);
#4845=ORIENTED_EDGE('',*,*,#3603,.F.);
#4846=ORIENTED_EDGE('',*,*,#3604,.T.);
#4847=ORIENTED_EDGE('',*,*,#3605,.F.);
#4848=ORIENTED_EDGE('',*,*,#3604,.F.);
#4849=ORIENTED_EDGE('',*,*,#3606,.F.);
#4850=ORIENTED_EDGE('',*,*,#3607,.F.);
#4851=ORIENTED_EDGE('',*,*,#3608,.F.);
#4852=ORIENTED_EDGE('',*,*,#3607,.T.);
#4853=ORIENTED_EDGE('',*,*,#3609,.T.);
#4854=ORIENTED_EDGE('',*,*,#3599,.T.);
#4855=ORIENTED_EDGE('',*,*,#3609,.F.);
#4856=ORIENTED_EDGE('',*,*,#3606,.T.);
#4857=ORIENTED_EDGE('',*,*,#3603,.T.);
#4858=ORIENTED_EDGE('',*,*,#3600,.T.);
#4859=ORIENTED_EDGE('',*,*,#3610,.F.);
#4860=ORIENTED_EDGE('',*,*,#3611,.T.);
#4861=ORIENTED_EDGE('',*,*,#3612,.F.);
#4862=ORIENTED_EDGE('',*,*,#3613,.T.);
#4863=ORIENTED_EDGE('',*,*,#3610,.T.);
#4864=ORIENTED_EDGE('',*,*,#3613,.F.);
#4865=ORIENTED_EDGE('',*,*,#3612,.T.);
#4866=ORIENTED_EDGE('',*,*,#3614,.F.);
#4867=ORIENTED_EDGE('',*,*,#3615,.F.);
#4868=ORIENTED_EDGE('',*,*,#3616,.T.);
#4869=ORIENTED_EDGE('',*,*,#3614,.T.);
#4870=ORIENTED_EDGE('',*,*,#3616,.F.);
#4871=ORIENTED_EDGE('',*,*,#3617,.F.);
#4872=ORIENTED_EDGE('',*,*,#3615,.T.);
#4873=ORIENTED_EDGE('',*,*,#3618,.F.);
#4874=ORIENTED_EDGE('',*,*,#3619,.T.);
#4875=ORIENTED_EDGE('',*,*,#3617,.T.);
#4876=ORIENTED_EDGE('',*,*,#3619,.F.);
#4877=ORIENTED_EDGE('',*,*,#3618,.T.);
#4878=ORIENTED_EDGE('',*,*,#3620,.F.);
#4879=ORIENTED_EDGE('',*,*,#3621,.F.);
#4880=ORIENTED_EDGE('',*,*,#3622,.T.);
#4881=ORIENTED_EDGE('',*,*,#3620,.T.);
#4882=ORIENTED_EDGE('',*,*,#3622,.F.);
#4883=ORIENTED_EDGE('',*,*,#3623,.F.);
#4884=ORIENTED_EDGE('',*,*,#3621,.T.);
#4885=ORIENTED_EDGE('',*,*,#3624,.F.);
#4886=ORIENTED_EDGE('',*,*,#3625,.T.);
#4887=ORIENTED_EDGE('',*,*,#3623,.T.);
#4888=ORIENTED_EDGE('',*,*,#3625,.F.);
#4889=ORIENTED_EDGE('',*,*,#3624,.T.);
#4890=ORIENTED_EDGE('',*,*,#3626,.F.);
#4891=ORIENTED_EDGE('',*,*,#3626,.T.);
#4892=ORIENTED_EDGE('',*,*,#3627,.T.);
#4893=ORIENTED_EDGE('',*,*,#3611,.F.);
#4894=ORIENTED_EDGE('',*,*,#3627,.F.);
#4895=ORIENTED_EDGE('',*,*,#3605,.T.);
#4896=ORIENTED_EDGE('',*,*,#3608,.T.);
#4897=ORIENTED_EDGE('',*,*,#3598,.T.);
#4898=ORIENTED_EDGE('',*,*,#3602,.T.);
#4899=ORIENTED_EDGE('',*,*,#3628,.F.);
#4900=ORIENTED_EDGE('',*,*,#3629,.F.);
#4901=ORIENTED_EDGE('',*,*,#3630,.F.);
#4902=ORIENTED_EDGE('',*,*,#3631,.F.);
#4903=ORIENTED_EDGE('',*,*,#3632,.F.);
#4904=ORIENTED_EDGE('',*,*,#3631,.T.);
#4905=ORIENTED_EDGE('',*,*,#3633,.F.);
#4906=ORIENTED_EDGE('',*,*,#3634,.T.);
#4907=ORIENTED_EDGE('',*,*,#3635,.F.);
#4908=ORIENTED_EDGE('',*,*,#3634,.F.);
#4909=ORIENTED_EDGE('',*,*,#3636,.F.);
#4910=ORIENTED_EDGE('',*,*,#3637,.F.);
#4911=ORIENTED_EDGE('',*,*,#3638,.F.);
#4912=ORIENTED_EDGE('',*,*,#3637,.T.);
#4913=ORIENTED_EDGE('',*,*,#3639,.F.);
#4914=ORIENTED_EDGE('',*,*,#3629,.T.);
#4915=ORIENTED_EDGE('',*,*,#3640,.F.);
#4916=ORIENTED_EDGE('',*,*,#3641,.T.);
#4917=ORIENTED_EDGE('',*,*,#3642,.F.);
#4918=ORIENTED_EDGE('',*,*,#3643,.T.);
#4919=ORIENTED_EDGE('',*,*,#3640,.T.);
#4920=ORIENTED_EDGE('',*,*,#3643,.F.);
#4921=ORIENTED_EDGE('',*,*,#3635,.T.);
#4922=ORIENTED_EDGE('',*,*,#3638,.T.);
#4923=ORIENTED_EDGE('',*,*,#3628,.T.);
#4924=ORIENTED_EDGE('',*,*,#3632,.T.);
#4925=ORIENTED_EDGE('',*,*,#3642,.T.);
#4926=ORIENTED_EDGE('',*,*,#3644,.F.);
#4927=ORIENTED_EDGE('',*,*,#3644,.T.);
#4928=ORIENTED_EDGE('',*,*,#3645,.T.);
#4929=ORIENTED_EDGE('',*,*,#3641,.F.);
#4930=ORIENTED_EDGE('',*,*,#3645,.F.);
#4931=ORIENTED_EDGE('',*,*,#3636,.T.);
#4932=ORIENTED_EDGE('',*,*,#3633,.T.);
#4933=ORIENTED_EDGE('',*,*,#3630,.T.);
#4934=ORIENTED_EDGE('',*,*,#3639,.T.);
#4935=ORIENTED_EDGE('',*,*,#3646,.F.);
#4936=ORIENTED_EDGE('',*,*,#3647,.T.);
#4937=ORIENTED_EDGE('',*,*,#3648,.F.);
#4938=ORIENTED_EDGE('',*,*,#3647,.F.);
#4939=ORIENTED_EDGE('',*,*,#3649,.F.);
#4940=ORIENTED_EDGE('',*,*,#3650,.T.);
#4941=ORIENTED_EDGE('',*,*,#3651,.F.);
#4942=ORIENTED_EDGE('',*,*,#3650,.F.);
#4943=ORIENTED_EDGE('',*,*,#3652,.F.);
#4944=ORIENTED_EDGE('',*,*,#3653,.T.);
#4945=ORIENTED_EDGE('',*,*,#3654,.F.);
#4946=ORIENTED_EDGE('',*,*,#3653,.F.);
#4947=ORIENTED_EDGE('',*,*,#3655,.F.);
#4948=ORIENTED_EDGE('',*,*,#3656,.T.);
#4949=ORIENTED_EDGE('',*,*,#3657,.F.);
#4950=ORIENTED_EDGE('',*,*,#3656,.F.);
#4951=ORIENTED_EDGE('',*,*,#3658,.F.);
#4952=ORIENTED_EDGE('',*,*,#3659,.T.);
#4953=ORIENTED_EDGE('',*,*,#3660,.F.);
#4954=ORIENTED_EDGE('',*,*,#3659,.F.);
#4955=ORIENTED_EDGE('',*,*,#3661,.T.);
#4956=ORIENTED_EDGE('',*,*,#3662,.T.);
#4957=ORIENTED_EDGE('',*,*,#3663,.F.);
#4958=ORIENTED_EDGE('',*,*,#3664,.F.);
#4959=ORIENTED_EDGE('',*,*,#3665,.T.);
#4960=ORIENTED_EDGE('',*,*,#3664,.T.);
#4961=ORIENTED_EDGE('',*,*,#3666,.F.);
#4962=ORIENTED_EDGE('',*,*,#3667,.F.);
#4963=ORIENTED_EDGE('',*,*,#3660,.T.);
#4964=ORIENTED_EDGE('',*,*,#3657,.T.);
#4965=ORIENTED_EDGE('',*,*,#3654,.T.);
#4966=ORIENTED_EDGE('',*,*,#3651,.T.);
#4967=ORIENTED_EDGE('',*,*,#3648,.T.);
#4968=ORIENTED_EDGE('',*,*,#3668,.T.);
#4969=ORIENTED_EDGE('',*,*,#3667,.T.);
#4970=ORIENTED_EDGE('',*,*,#3669,.F.);
#4971=ORIENTED_EDGE('',*,*,#3670,.F.);
#4972=ORIENTED_EDGE('',*,*,#3671,.T.);
#4973=ORIENTED_EDGE('',*,*,#3670,.T.);
#4974=ORIENTED_EDGE('',*,*,#3672,.F.);
#4975=ORIENTED_EDGE('',*,*,#3662,.F.);
#4976=ORIENTED_EDGE('',*,*,#3658,.T.);
#4977=ORIENTED_EDGE('',*,*,#3655,.T.);
#4978=ORIENTED_EDGE('',*,*,#3652,.T.);
#4979=ORIENTED_EDGE('',*,*,#3649,.T.);
#4980=ORIENTED_EDGE('',*,*,#3646,.T.);
#4981=ORIENTED_EDGE('',*,*,#3672,.T.);
#4982=ORIENTED_EDGE('',*,*,#3669,.T.);
#4983=ORIENTED_EDGE('',*,*,#3666,.T.);
#4984=ORIENTED_EDGE('',*,*,#3663,.T.);
#4985=ORIENTED_EDGE('',*,*,#3671,.F.);
#4986=ORIENTED_EDGE('',*,*,#3661,.F.);
#4987=ORIENTED_EDGE('',*,*,#3665,.F.);
#4988=ORIENTED_EDGE('',*,*,#3668,.F.);
#4989=ORIENTED_EDGE('',*,*,#3673,.F.);
#4990=ORIENTED_EDGE('',*,*,#3674,.T.);
#4991=ORIENTED_EDGE('',*,*,#3675,.T.);
#4992=ORIENTED_EDGE('',*,*,#3674,.F.);
#4993=ORIENTED_EDGE('',*,*,#3676,.F.);
#4994=ORIENTED_EDGE('',*,*,#3677,.T.);
#4995=ORIENTED_EDGE('',*,*,#3678,.T.);
#4996=ORIENTED_EDGE('',*,*,#3677,.F.);
#4997=ORIENTED_EDGE('',*,*,#3676,.T.);
#4998=ORIENTED_EDGE('',*,*,#3673,.T.);
#4999=ORIENTED_EDGE('',*,*,#3678,.F.);
#5000=ORIENTED_EDGE('',*,*,#3675,.F.);
#5001=ORIENTED_EDGE('',*,*,#3679,.F.);
#5002=ORIENTED_EDGE('',*,*,#3680,.T.);
#5003=ORIENTED_EDGE('',*,*,#3681,.T.);
#5004=ORIENTED_EDGE('',*,*,#3680,.F.);
#5005=ORIENTED_EDGE('',*,*,#3682,.F.);
#5006=ORIENTED_EDGE('',*,*,#3683,.T.);
#5007=ORIENTED_EDGE('',*,*,#3684,.T.);
#5008=ORIENTED_EDGE('',*,*,#3683,.F.);
#5009=ORIENTED_EDGE('',*,*,#3682,.T.);
#5010=ORIENTED_EDGE('',*,*,#3679,.T.);
#5011=ORIENTED_EDGE('',*,*,#3684,.F.);
#5012=ORIENTED_EDGE('',*,*,#3681,.F.);
#5013=ORIENTED_EDGE('',*,*,#3685,.T.);
#5014=ORIENTED_EDGE('',*,*,#3686,.T.);
#5015=ORIENTED_EDGE('',*,*,#3687,.T.);
#5016=ORIENTED_EDGE('',*,*,#3688,.F.);
#5017=ORIENTED_EDGE('',*,*,#3689,.T.);
#5018=ORIENTED_EDGE('',*,*,#3690,.T.);
#5019=ORIENTED_EDGE('',*,*,#3691,.T.);
#5020=ORIENTED_EDGE('',*,*,#3686,.F.);
#5021=ORIENTED_EDGE('',*,*,#3692,.T.);
#5022=ORIENTED_EDGE('',*,*,#3693,.T.);
#5023=ORIENTED_EDGE('',*,*,#3694,.T.);
#5024=ORIENTED_EDGE('',*,*,#3690,.F.);
#5025=ORIENTED_EDGE('',*,*,#3695,.T.);
#5026=ORIENTED_EDGE('',*,*,#3696,.T.);
#5027=ORIENTED_EDGE('',*,*,#3697,.T.);
#5028=ORIENTED_EDGE('',*,*,#3693,.F.);
#5029=ORIENTED_EDGE('',*,*,#3698,.T.);
#5030=ORIENTED_EDGE('',*,*,#3699,.T.);
#5031=ORIENTED_EDGE('',*,*,#3700,.T.);
#5032=ORIENTED_EDGE('',*,*,#3696,.F.);
#5033=ORIENTED_EDGE('',*,*,#3701,.T.);
#5034=ORIENTED_EDGE('',*,*,#3688,.T.);
#5035=ORIENTED_EDGE('',*,*,#3702,.T.);
#5036=ORIENTED_EDGE('',*,*,#3699,.F.);
#5037=ORIENTED_EDGE('',*,*,#3701,.F.);
#5038=ORIENTED_EDGE('',*,*,#3698,.F.);
#5039=ORIENTED_EDGE('',*,*,#3695,.F.);
#5040=ORIENTED_EDGE('',*,*,#3692,.F.);
#5041=ORIENTED_EDGE('',*,*,#3689,.F.);
#5042=ORIENTED_EDGE('',*,*,#3685,.F.);
#5043=ORIENTED_EDGE('',*,*,#3702,.F.);
#5044=ORIENTED_EDGE('',*,*,#3687,.F.);
#5045=ORIENTED_EDGE('',*,*,#3691,.F.);
#5046=ORIENTED_EDGE('',*,*,#3694,.F.);
#5047=ORIENTED_EDGE('',*,*,#3697,.F.);
#5048=ORIENTED_EDGE('',*,*,#3700,.F.);
#5049=ORIENTED_EDGE('',*,*,#3703,.F.);
#5050=ORIENTED_EDGE('',*,*,#3704,.F.);
#5051=ORIENTED_EDGE('',*,*,#3705,.F.);
#5052=ORIENTED_EDGE('',*,*,#3706,.T.);
#5053=ORIENTED_EDGE('',*,*,#3704,.T.);
#5054=ORIENTED_EDGE('',*,*,#3706,.F.);
#5055=ORIENTED_EDGE('',*,*,#3707,.F.);
#5056=ORIENTED_EDGE('',*,*,#3708,.T.);
#5057=ORIENTED_EDGE('',*,*,#3705,.T.);
#5058=ORIENTED_EDGE('',*,*,#3708,.F.);
#5059=ORIENTED_EDGE('',*,*,#3709,.F.);
#5060=ORIENTED_EDGE('',*,*,#3710,.T.);
#5061=ORIENTED_EDGE('',*,*,#3707,.T.);
#5062=ORIENTED_EDGE('',*,*,#3710,.F.);
#5063=ORIENTED_EDGE('',*,*,#3709,.T.);
#5064=ORIENTED_EDGE('',*,*,#3711,.F.);
#5065=ORIENTED_EDGE('',*,*,#3712,.F.);
#5066=ORIENTED_EDGE('',*,*,#3713,.T.);
#5067=ORIENTED_EDGE('',*,*,#3711,.T.);
#5068=ORIENTED_EDGE('',*,*,#3713,.F.);
#5069=ORIENTED_EDGE('',*,*,#3703,.T.);
#5070=ORIENTED_EDGE('',*,*,#3714,.T.);
#5071=ORIENTED_EDGE('',*,*,#3712,.T.);
#5072=ORIENTED_EDGE('',*,*,#3714,.F.);
#5073=CYLINDRICAL_SURFACE('',#5918,0.164999999999999);
#5074=CYLINDRICAL_SURFACE('',#5921,0.164999999999999);
#5075=CYLINDRICAL_SURFACE('',#5924,0.165);
#5076=CYLINDRICAL_SURFACE('',#5927,0.165);
#5077=CYLINDRICAL_SURFACE('',#5930,0.21);
#5078=CYLINDRICAL_SURFACE('',#5933,0.21);
#5079=CYLINDRICAL_SURFACE('',#5936,0.21);
#5080=CYLINDRICAL_SURFACE('',#5939,0.21);
#5081=CYLINDRICAL_SURFACE('',#5963,0.425);
#5082=CYLINDRICAL_SURFACE('',#5971,0.24505);
#5083=CYLINDRICAL_SURFACE('',#5973,0.25);
#5084=CYLINDRICAL_SURFACE('',#5974,0.165);
#5085=CYLINDRICAL_SURFACE('',#5978,0.165);
#5086=CYLINDRICAL_SURFACE('',#5982,0.165);
#5087=CYLINDRICAL_SURFACE('',#5986,0.165);
#5088=CYLINDRICAL_SURFACE('',#5993,0.525);
#5089=CYLINDRICAL_SURFACE('',#5995,0.525);
#5090=CYLINDRICAL_SURFACE('',#6000,0.525);
#5091=CYLINDRICAL_SURFACE('',#6005,0.525);
#5092=CYLINDRICAL_SURFACE('',#6010,2.2);
#5093=CYLINDRICAL_SURFACE('',#6023,0.275);
#5094=CYLINDRICAL_SURFACE('',#6025,0.275);
#5095=CYLINDRICAL_SURFACE('',#6027,0.275);
#5096=CYLINDRICAL_SURFACE('',#6029,0.275);
#5097=CYLINDRICAL_SURFACE('',#6031,1.5);
#5098=CYLINDRICAL_SURFACE('',#6036,3.);
#5099=CYLINDRICAL_SURFACE('',#6038,1.02);
#5100=CYLINDRICAL_SURFACE('',#6043,0.375);
#5101=CYLINDRICAL_SURFACE('',#6048,0.375);
#5102=CYLINDRICAL_SURFACE('',#6053,0.375);
#5103=CYLINDRICAL_SURFACE('',#6058,0.375);
#5104=CYLINDRICAL_SURFACE('',#6063,0.225);
#5105=CYLINDRICAL_SURFACE('',#6065,0.225);
#5106=CYLINDRICAL_SURFACE('',#6067,0.225);
#5107=CYLINDRICAL_SURFACE('',#6069,0.225);
#5108=CYLINDRICAL_SURFACE('',#6071,1.49);
#5109=CYLINDRICAL_SURFACE('',#6076,0.71);
#5110=CYLINDRICAL_SURFACE('',#6078,2.2);
#5111=CYLINDRICAL_SURFACE('',#6091,0.976185);
#5112=CYLINDRICAL_SURFACE('',#6093,0.5);
#5113=CYLINDRICAL_SURFACE('',#6099,0.976185);
#5114=CYLINDRICAL_SURFACE('',#6111,1.023815);
#5115=CYLINDRICAL_SURFACE('',#6118,1.5);
#5116=CYLINDRICAL_SURFACE('',#6123,1.023815);
#5117=CYLINDRICAL_SURFACE('',#6145,1.019052);
#5118=CYLINDRICAL_SURFACE('',#6185,0.980948);
#5119=CYLINDRICAL_SURFACE('',#6199,1.013815);
#5120=CYLINDRICAL_SURFACE('',#6203,0.991185);
#5121=CYLINDRICAL_SURFACE('',#6207,1.013815);
#5122=CYLINDRICAL_SURFACE('',#6211,0.991185);
#5123=CYLINDRICAL_SURFACE('',#6223,0.6);
#5124=CYLINDRICAL_SURFACE('',#6230,0.165);
#5125=CYLINDRICAL_SURFACE('',#6234,0.4);
#5126=CYLINDRICAL_SURFACE('',#6239,0.4);
#5127=CYLINDRICAL_SURFACE('',#6245,0.225);
#5128=CYLINDRICAL_SURFACE('',#6247,0.225);
#5129=CYLINDRICAL_SURFACE('',#6249,0.6);
#5130=CYLINDRICAL_SURFACE('',#6267,0.1954);
#5131=CYLINDRICAL_SURFACE('',#6274,0.25);
#5132=CYLINDRICAL_SURFACE('',#6277,0.25);
#5133=CYLINDRICAL_SURFACE('',#6280,0.225);
#5134=CYLINDRICAL_SURFACE('',#6283,0.8);
#5135=CYLINDRICAL_SURFACE('',#6294,1.);
#5136=CYLINDRICAL_SURFACE('',#6296,1.);
#5137=CYLINDRICAL_SURFACE('',#6298,0.8);
#5138=CYLINDRICAL_SURFACE('',#6306,0.8);
#5139=CYLINDRICAL_SURFACE('',#6309,1.);
#5140=CYLINDRICAL_SURFACE('',#6313,0.7);
#5141=CYLINDRICAL_SURFACE('',#6314,0.5);
#5142=CYLINDRICAL_SURFACE('',#6318,0.165);
#5143=CYLINDRICAL_SURFACE('',#6322,0.6);
#5144=CYLINDRICAL_SURFACE('',#6328,0.505);
#5145=CYLINDRICAL_SURFACE('',#6331,0.7);
#5146=CYLINDRICAL_SURFACE('',#6339,0.165);
#5147=CYLINDRICAL_SURFACE('',#6342,0.505);
#5148=CYLINDRICAL_SURFACE('',#6345,0.9);
#5149=CYLINDRICAL_SURFACE('',#6355,0.35);
#5150=CYLINDRICAL_SURFACE('',#6363,0.1954);
#5151=CYLINDRICAL_SURFACE('',#6390,0.1954);
#5152=CYLINDRICAL_SURFACE('',#6392,0.165);
#5153=CYLINDRICAL_SURFACE('',#6402,0.7);
#5154=CYLINDRICAL_SURFACE('',#6403,0.3);
#5155=CYLINDRICAL_SURFACE('',#6405,0.3);
#5156=CYLINDRICAL_SURFACE('',#6410,0.305);
#5157=CYLINDRICAL_SURFACE('',#6413,0.5);
#5158=CYLINDRICAL_SURFACE('',#6420,0.5);
#5159=CYLINDRICAL_SURFACE('',#6423,0.5);
#5160=CYLINDRICAL_SURFACE('',#6426,0.800000000000001);
#5161=CYLINDRICAL_SURFACE('',#6433,0.8);
#5162=CYLINDRICAL_SURFACE('',#6437,0.305);
#5163=CYLINDRICAL_SURFACE('',#6440,0.5);
#5164=CYLINDRICAL_SURFACE('',#6450,0.165);
#5165=CYLINDRICAL_SURFACE('',#6460,0.699999999999999);
#5166=CYLINDRICAL_SURFACE('',#6461,0.3);
#5167=CYLINDRICAL_SURFACE('',#6463,0.3);
#5168=CYLINDRICAL_SURFACE('',#6468,0.305);
#5169=CYLINDRICAL_SURFACE('',#6471,0.5);
#5170=CYLINDRICAL_SURFACE('',#6477,0.25);
#5171=CYLINDRICAL_SURFACE('',#6481,0.165);
#5172=CYLINDRICAL_SURFACE('',#6484,0.165);
#5173=CYLINDRICAL_SURFACE('',#6487,0.165);
#5174=CYLINDRICAL_SURFACE('',#6490,0.165);
#5175=CYLINDRICAL_SURFACE('',#6493,1.05);
#5176=CYLINDRICAL_SURFACE('',#6514,1.05);
#5177=CYLINDRICAL_SURFACE('',#6518,1.);
#5178=CYLINDRICAL_SURFACE('',#6522,1.05);
#5179=CYLINDRICAL_SURFACE('',#6526,1.);
#5180=CYLINDRICAL_SURFACE('',#6530,1.05);
#5181=CYLINDRICAL_SURFACE('',#6534,0.9);
#5182=CYLINDRICAL_SURFACE('',#6547,0.895);
#5183=CYLINDRICAL_SURFACE('',#6551,0.605);
#5184=CYLINDRICAL_SURFACE('',#6555,0.225);
#5185=CYLINDRICAL_SURFACE('',#6558,0.225);
#5186=CYLINDRICAL_SURFACE('',#6561,0.225);
#5187=CYLINDRICAL_SURFACE('',#6564,0.225);
#5188=CYLINDRICAL_SURFACE('',#6567,0.7);
#5189=CYLINDRICAL_SURFACE('',#6577,0.305);
#5190=CYLINDRICAL_SURFACE('',#6580,0.5);
#5191=CYLINDRICAL_SURFACE('',#6586,0.225);
#5192=CYLINDRICAL_SURFACE('',#6589,0.5);
#5193=CYLINDRICAL_SURFACE('',#6609,0.35);
#5194=CYLINDRICAL_SURFACE('',#6617,0.1954);
#5195=ADVANCED_FACE('',(#790),#5073,.F.);
#5196=ADVANCED_FACE('',(#791),#5074,.F.);
#5197=ADVANCED_FACE('',(#792),#5075,.F.);
#5198=ADVANCED_FACE('',(#793),#5076,.F.);
#5199=ADVANCED_FACE('',(#794),#5077,.F.);
#5200=ADVANCED_FACE('',(#795),#5078,.F.);
#5201=ADVANCED_FACE('',(#796),#5079,.F.);
#5202=ADVANCED_FACE('',(#797),#5080,.F.);
#5203=ADVANCED_FACE('',(#798),#612,.T.);
#5204=ADVANCED_FACE('',(#799),#613,.T.);
#5205=ADVANCED_FACE('',(#800),#614,.T.);
#5206=ADVANCED_FACE('',(#801),#615,.T.);
#5207=ADVANCED_FACE('',(#802,#473,#474,#475,#476,#477,#478,#479,#480),#616,
 .T.);
#5208=ADVANCED_FACE('',(#803,#481,#482,#483,#484,#485,#486,#487,#488),#617,
 .F.);
#5209=ADVANCED_FACE('',(#804),#618,.F.);
#5210=ADVANCED_FACE('',(#805),#619,.F.);
#5211=ADVANCED_FACE('',(#806),#620,.F.);
#5212=ADVANCED_FACE('',(#807),#621,.F.);
#5213=ADVANCED_FACE('',(#808),#622,.F.);
#5214=ADVANCED_FACE('',(#809),#623,.F.);
#5215=ADVANCED_FACE('',(#810),#624,.F.);
#5216=ADVANCED_FACE('',(#811),#625,.F.);
#5217=ADVANCED_FACE('',(#812),#626,.F.);
#5218=ADVANCED_FACE('',(#813),#627,.T.);
#5219=ADVANCED_FACE('',(#814),#312,.T.);
#5220=ADVANCED_FACE('',(#815),#5081,.T.);
#5221=ADVANCED_FACE('',(#816),#313,.T.);
#5222=ADVANCED_FACE('',(#817,#489),#628,.T.);
#5223=ADVANCED_FACE('',(#818),#314,.T.);
#5224=ADVANCED_FACE('',(#819),#5082,.T.);
#5225=ADVANCED_FACE('',(#820),#5083,.F.);
#5226=ADVANCED_FACE('',(#821),#5084,.F.);
#5227=ADVANCED_FACE('',(#822),#629,.T.);
#5228=ADVANCED_FACE('',(#823),#5085,.F.);
#5229=ADVANCED_FACE('',(#824),#630,.T.);
#5230=ADVANCED_FACE('',(#825),#5086,.F.);
#5231=ADVANCED_FACE('',(#826),#631,.T.);
#5232=ADVANCED_FACE('',(#827),#5087,.F.);
#5233=ADVANCED_FACE('',(#828),#632,.T.);
#5234=ADVANCED_FACE('',(#829),#633,.F.);
#5235=ADVANCED_FACE('',(#830),#5088,.F.);
#5236=ADVANCED_FACE('',(#831),#5089,.F.);
#5237=ADVANCED_FACE('',(#832),#634,.F.);
#5238=ADVANCED_FACE('',(#833),#5090,.F.);
#5239=ADVANCED_FACE('',(#834),#635,.F.);
#5240=ADVANCED_FACE('',(#835),#5091,.F.);
#5241=ADVANCED_FACE('',(#836),#636,.F.);
#5242=ADVANCED_FACE('',(#837),#5092,.T.);
#5243=ADVANCED_FACE('',(#838,#490,#491,#492,#493,#494),#637,.T.);
#5244=ADVANCED_FACE('',(#839),#5093,.F.);
#5245=ADVANCED_FACE('',(#840),#5094,.F.);
#5246=ADVANCED_FACE('',(#841),#5095,.F.);
#5247=ADVANCED_FACE('',(#842),#5096,.F.);
#5248=ADVANCED_FACE('',(#843),#5097,.F.);
#5249=ADVANCED_FACE('',(#844,#495),#638,.T.);
#5250=ADVANCED_FACE('',(#845,#496),#5098,.T.);
#5251=ADVANCED_FACE('',(#846,#497),#5099,.F.);
#5252=ADVANCED_FACE('',(#847,#498,#499,#500,#501,#502),#639,.T.);
#5253=ADVANCED_FACE('',(#848,#503,#504,#505,#506,#507),#640,.F.);
#5254=ADVANCED_FACE('',(#849),#5100,.F.);
#5255=ADVANCED_FACE('',(#850,#508),#641,.T.);
#5256=ADVANCED_FACE('',(#851),#5101,.F.);
#5257=ADVANCED_FACE('',(#852,#509),#642,.T.);
#5258=ADVANCED_FACE('',(#853),#5102,.F.);
#5259=ADVANCED_FACE('',(#854,#510),#643,.T.);
#5260=ADVANCED_FACE('',(#855),#5103,.F.);
#5261=ADVANCED_FACE('',(#856,#511),#644,.T.);
#5262=ADVANCED_FACE('',(#857),#5104,.F.);
#5263=ADVANCED_FACE('',(#858),#5105,.F.);
#5264=ADVANCED_FACE('',(#859),#5106,.F.);
#5265=ADVANCED_FACE('',(#860),#5107,.F.);
#5266=ADVANCED_FACE('',(#861),#5108,.T.);
#5267=ADVANCED_FACE('',(#862,#512),#645,.F.);
#5268=ADVANCED_FACE('',(#863),#5109,.F.);
#5269=ADVANCED_FACE('',(#864),#5110,.T.);
#5270=ADVANCED_FACE('',(#865,#513,#514,#515,#516,#517),#646,.T.);
#5271=ADVANCED_FACE('',(#866,#518,#519,#520,#521,#522),#647,.F.);
#5272=ADVANCED_FACE('',(#867),#279,.F.);
#5273=ADVANCED_FACE('',(#868),#5111,.T.);
#5274=ADVANCED_FACE('',(#869),#5112,.F.);
#5275=ADVANCED_FACE('',(#870),#315,.F.);
#5276=ADVANCED_FACE('',(#871,#523),#648,.T.);
#5277=ADVANCED_FACE('',(#872),#5113,.T.);
#5278=ADVANCED_FACE('',(#873,#524),#649,.T.);
#5279=ADVANCED_FACE('',(#874),#316,.F.);
#5280=ADVANCED_FACE('',(#875),#280,.F.);
#5281=ADVANCED_FACE('',(#876),#5114,.F.);
#5282=ADVANCED_FACE('',(#877,#525),#650,.T.);
#5283=ADVANCED_FACE('',(#878),#317,.T.);
#5284=ADVANCED_FACE('',(#879),#5115,.T.);
#5285=ADVANCED_FACE('',(#880),#318,.T.);
#5286=ADVANCED_FACE('',(#881,#526),#651,.T.);
#5287=ADVANCED_FACE('',(#882),#5116,.F.);
#5288=ADVANCED_FACE('',(#883),#263,.T.);
#5289=ADVANCED_FACE('',(#884),#264,.T.);
#5290=ADVANCED_FACE('',(#885),#265,.T.);
#5291=ADVANCED_FACE('',(#886),#266,.T.);
#5292=ADVANCED_FACE('',(#887),#267,.T.);
#5293=ADVANCED_FACE('',(#888),#268,.T.);
#5294=ADVANCED_FACE('',(#889),#269,.T.);
#5295=ADVANCED_FACE('',(#890),#270,.T.);
#5296=ADVANCED_FACE('',(#891),#271,.F.);
#5297=ADVANCED_FACE('',(#892),#5117,.T.);
#5298=ADVANCED_FACE('',(#893),#652,.T.);
#5299=ADVANCED_FACE('',(#894),#272,.F.);
#5300=ADVANCED_FACE('',(#895),#653,.T.);
#5301=ADVANCED_FACE('',(#896),#273,.F.);
#5302=ADVANCED_FACE('',(#897),#654,.T.);
#5303=ADVANCED_FACE('',(#898),#274,.F.);
#5304=ADVANCED_FACE('',(#899),#655,.T.);
#5305=ADVANCED_FACE('',(#900),#275,.F.);
#5306=ADVANCED_FACE('',(#901),#656,.T.);
#5307=ADVANCED_FACE('',(#902),#276,.F.);
#5308=ADVANCED_FACE('',(#903),#657,.T.);
#5309=ADVANCED_FACE('',(#904),#277,.F.);
#5310=ADVANCED_FACE('',(#905),#5118,.F.);
#5311=ADVANCED_FACE('',(#906),#658,.T.);
#5312=ADVANCED_FACE('',(#907),#278,.F.);
#5313=ADVANCED_FACE('',(#908,#527),#659,.T.);
#5314=ADVANCED_FACE('',(#909),#660,.T.);
#5315=ADVANCED_FACE('',(#910,#528),#661,.T.);
#5316=ADVANCED_FACE('',(#911),#5119,.T.);
#5317=ADVANCED_FACE('',(#912,#529),#662,.T.);
#5318=ADVANCED_FACE('',(#913),#5120,.F.);
#5319=ADVANCED_FACE('',(#914,#530),#663,.T.);
#5320=ADVANCED_FACE('',(#915),#5121,.T.);
#5321=ADVANCED_FACE('',(#916,#531),#664,.T.);
#5322=ADVANCED_FACE('',(#917),#5122,.F.);
#5323=ADVANCED_FACE('',(#918),#665,.T.);
#5324=ADVANCED_FACE('',(#919),#319,.T.);
#5325=ADVANCED_FACE('',(#920),#5123,.T.);
#5326=ADVANCED_FACE('',(#921),#666,.F.);
#5327=ADVANCED_FACE('',(#922),#667,.T.);
#5328=ADVANCED_FACE('',(#923),#668,.T.);
#5329=ADVANCED_FACE('',(#924),#669,.T.);
#5330=ADVANCED_FACE('',(#925),#5124,.F.);
#5331=ADVANCED_FACE('',(#926),#670,.T.);
#5332=ADVANCED_FACE('',(#927),#5125,.F.);
#5333=ADVANCED_FACE('',(#928,#532),#671,.T.);
#5334=ADVANCED_FACE('',(#929),#5126,.F.);
#5335=ADVANCED_FACE('',(#930,#533),#672,.T.);
#5336=ADVANCED_FACE('',(#931,#534,#535,#536),#673,.T.);
#5337=ADVANCED_FACE('',(#932),#5127,.F.);
#5338=ADVANCED_FACE('',(#933),#5128,.F.);
#5339=ADVANCED_FACE('',(#934),#5129,.F.);
#5340=ADVANCED_FACE('',(#935,#537),#674,.T.);
#5341=ADVANCED_FACE('',(#936,#538),#675,.T.);
#5342=ADVANCED_FACE('',(#937,#539,#540),#676,.F.);
#5343=ADVANCED_FACE('',(#938),#677,.F.);
#5344=ADVANCED_FACE('',(#939),#678,.F.);
#5345=ADVANCED_FACE('',(#940),#679,.F.);
#5346=ADVANCED_FACE('',(#941),#680,.F.);
#5347=ADVANCED_FACE('',(#942),#681,.F.);
#5348=ADVANCED_FACE('',(#943),#682,.F.);
#5349=ADVANCED_FACE('',(#944),#683,.F.);
#5350=ADVANCED_FACE('',(#945,#541),#684,.T.);
#5351=ADVANCED_FACE('',(#946),#320,.T.);
#5352=ADVANCED_FACE('',(#947),#5130,.T.);
#5353=ADVANCED_FACE('',(#948),#321,.T.);
#5354=ADVANCED_FACE('',(#949),#685,.T.);
#5355=ADVANCED_FACE('',(#950),#5131,.F.);
#5356=ADVANCED_FACE('',(#951),#5132,.F.);
#5357=ADVANCED_FACE('',(#952),#5133,.F.);
#5358=ADVANCED_FACE('',(#953),#5134,.T.);
#5359=ADVANCED_FACE('',(#954),#686,.T.);
#5360=ADVANCED_FACE('',(#955,#542,#543,#544),#687,.T.);
#5361=ADVANCED_FACE('',(#956),#688,.T.);
#5362=ADVANCED_FACE('',(#957),#5135,.T.);
#5363=ADVANCED_FACE('',(#958),#5136,.T.);
#5364=ADVANCED_FACE('',(#959),#5137,.T.);
#5365=ADVANCED_FACE('',(#960),#689,.T.);
#5366=ADVANCED_FACE('',(#961,#545,#546,#547,#548),#690,.F.);
#5367=ADVANCED_FACE('',(#962),#691,.T.);
#5368=ADVANCED_FACE('',(#963),#5138,.T.);
#5369=ADVANCED_FACE('',(#964),#692,.T.);
#5370=ADVANCED_FACE('',(#965),#693,.T.);
#5371=ADVANCED_FACE('',(#966),#5139,.T.);
#5372=ADVANCED_FACE('',(#967,#549),#694,.F.);
#5373=ADVANCED_FACE('',(#968),#5140,.T.);
#5374=ADVANCED_FACE('',(#969),#5141,.T.);
#5375=ADVANCED_FACE('',(#970),#695,.F.);
#5376=ADVANCED_FACE('',(#971),#5142,.F.);
#5377=ADVANCED_FACE('',(#972),#696,.F.);
#5378=ADVANCED_FACE('',(#973),#5143,.T.);
#5379=ADVANCED_FACE('',(#974),#697,.T.);
#5380=ADVANCED_FACE('',(#975,#550),#698,.F.);
#5381=ADVANCED_FACE('',(#976),#5144,.F.);
#5382=ADVANCED_FACE('',(#977),#5145,.T.);
#5383=ADVANCED_FACE('',(#978,#551),#699,.T.);
#5384=ADVANCED_FACE('',(#979,#552),#700,.F.);
#5385=ADVANCED_FACE('',(#980),#701,.T.);
#5386=ADVANCED_FACE('',(#981),#5146,.F.);
#5387=ADVANCED_FACE('',(#982),#702,.T.);
#5388=ADVANCED_FACE('',(#983,#553),#5147,.F.);
#5389=ADVANCED_FACE('',(#984,#554),#5148,.T.);
#5390=ADVANCED_FACE('',(#985,#555),#703,.T.);
#5391=ADVANCED_FACE('',(#986,#556),#704,.F.);
#5392=ADVANCED_FACE('',(#987),#705,.T.);
#5393=ADVANCED_FACE('',(#988),#322,.T.);
#5394=ADVANCED_FACE('',(#989),#5149,.T.);
#5395=ADVANCED_FACE('',(#990),#323,.T.);
#5396=ADVANCED_FACE('',(#991,#557),#706,.T.);
#5397=ADVANCED_FACE('',(#992),#324,.T.);
#5398=ADVANCED_FACE('',(#993),#5150,.T.);
#5399=ADVANCED_FACE('',(#994),#325,.T.);
#5400=ADVANCED_FACE('',(#995),#707,.T.);
#5401=ADVANCED_FACE('',(#996),#708,.F.);
#5402=ADVANCED_FACE('',(#997),#709,.F.);
#5403=ADVANCED_FACE('',(#998),#710,.F.);
#5404=ADVANCED_FACE('',(#999),#711,.F.);
#5405=ADVANCED_FACE('',(#1000),#712,.F.);
#5406=ADVANCED_FACE('',(#1001),#713,.F.);
#5407=ADVANCED_FACE('',(#1002),#714,.F.);
#5408=ADVANCED_FACE('',(#1003),#715,.F.);
#5409=ADVANCED_FACE('',(#1004),#716,.F.);
#5410=ADVANCED_FACE('',(#1005),#717,.F.);
#5411=ADVANCED_FACE('',(#1006),#718,.F.);
#5412=ADVANCED_FACE('',(#1007),#719,.F.);
#5413=ADVANCED_FACE('',(#1008),#720,.F.);
#5414=ADVANCED_FACE('',(#1009),#721,.F.);
#5415=ADVANCED_FACE('',(#1010),#722,.F.);
#5416=ADVANCED_FACE('',(#1011),#723,.F.);
#5417=ADVANCED_FACE('',(#1012,#558),#724,.T.);
#5418=ADVANCED_FACE('',(#1013),#326,.T.);
#5419=ADVANCED_FACE('',(#1014),#5151,.T.);
#5420=ADVANCED_FACE('',(#1015),#5152,.F.);
#5421=ADVANCED_FACE('',(#1016),#725,.T.);
#5422=ADVANCED_FACE('',(#1017,#559),#726,.T.);
#5423=ADVANCED_FACE('',(#1018,#560),#727,.F.);
#5424=ADVANCED_FACE('',(#1019),#5153,.T.);
#5425=ADVANCED_FACE('',(#1020),#5154,.T.);
#5426=ADVANCED_FACE('',(#1021),#5155,.T.);
#5427=ADVANCED_FACE('',(#1022,#561),#728,.T.);
#5428=ADVANCED_FACE('',(#1023),#729,.F.);
#5429=ADVANCED_FACE('',(#1024),#5156,.F.);
#5430=ADVANCED_FACE('',(#1025),#5157,.T.);
#5431=ADVANCED_FACE('',(#1026,#562),#730,.T.);
#5432=ADVANCED_FACE('',(#1027,#563),#731,.F.);
#5433=ADVANCED_FACE('',(#1028),#5158,.F.);
#5434=ADVANCED_FACE('',(#1029),#5159,.F.);
#5435=ADVANCED_FACE('',(#1030),#5160,.T.);
#5436=ADVANCED_FACE('',(#1031),#732,.T.);
#5437=ADVANCED_FACE('',(#1032,#564,#565),#733,.F.);
#5438=ADVANCED_FACE('',(#1033),#734,.T.);
#5439=ADVANCED_FACE('',(#1034),#5161,.T.);
#5440=ADVANCED_FACE('',(#1035,#566,#567),#735,.T.);
#5441=ADVANCED_FACE('',(#1036),#5162,.F.);
#5442=ADVANCED_FACE('',(#1037),#5163,.T.);
#5443=ADVANCED_FACE('',(#1038,#568),#736,.T.);
#5444=ADVANCED_FACE('',(#1039,#569),#737,.F.);
#5445=ADVANCED_FACE('',(#1040),#5164,.F.);
#5446=ADVANCED_FACE('',(#1041),#738,.T.);
#5447=ADVANCED_FACE('',(#1042,#570),#739,.T.);
#5448=ADVANCED_FACE('',(#1043,#571),#740,.F.);
#5449=ADVANCED_FACE('',(#1044),#5165,.T.);
#5450=ADVANCED_FACE('',(#1045),#5166,.T.);
#5451=ADVANCED_FACE('',(#1046),#5167,.T.);
#5452=ADVANCED_FACE('',(#1047,#572),#741,.T.);
#5453=ADVANCED_FACE('',(#1048),#742,.F.);
#5454=ADVANCED_FACE('',(#1049),#5168,.F.);
#5455=ADVANCED_FACE('',(#1050),#5169,.T.);
#5456=ADVANCED_FACE('',(#1051,#573),#743,.T.);
#5457=ADVANCED_FACE('',(#1052,#574),#744,.F.);
#5458=ADVANCED_FACE('',(#1053),#5170,.F.);
#5459=ADVANCED_FACE('',(#1054),#745,.T.);
#5460=ADVANCED_FACE('',(#1055),#5171,.F.);
#5461=ADVANCED_FACE('',(#1056),#5172,.F.);
#5462=ADVANCED_FACE('',(#1057),#5173,.F.);
#5463=ADVANCED_FACE('',(#1058),#5174,.F.);
#5464=ADVANCED_FACE('',(#1059),#5175,.F.);
#5465=ADVANCED_FACE('',(#1060),#746,.T.);
#5466=ADVANCED_FACE('',(#1061,#575,#576,#577,#578,#579),#747,.T.);
#5467=ADVANCED_FACE('',(#1062),#748,.T.);
#5468=ADVANCED_FACE('',(#1063,#580,#581,#582,#583,#584),#749,.T.);
#5469=ADVANCED_FACE('',(#1064,#585),#750,.T.);
#5470=ADVANCED_FACE('',(#1065),#751,.F.);
#5471=ADVANCED_FACE('',(#1066),#752,.F.);
#5472=ADVANCED_FACE('',(#1067),#753,.F.);
#5473=ADVANCED_FACE('',(#1068),#754,.F.);
#5474=ADVANCED_FACE('',(#1069),#755,.F.);
#5475=ADVANCED_FACE('',(#1070),#756,.F.);
#5476=ADVANCED_FACE('',(#1071,#586),#757,.T.);
#5477=ADVANCED_FACE('',(#1072),#5176,.T.);
#5478=ADVANCED_FACE('',(#1073,#587),#758,.T.);
#5479=ADVANCED_FACE('',(#1074),#5177,.T.);
#5480=ADVANCED_FACE('',(#1075,#588),#759,.T.);
#5481=ADVANCED_FACE('',(#1076),#5178,.T.);
#5482=ADVANCED_FACE('',(#1077,#589),#760,.T.);
#5483=ADVANCED_FACE('',(#1078),#5179,.T.);
#5484=ADVANCED_FACE('',(#1079,#590),#761,.T.);
#5485=ADVANCED_FACE('',(#1080),#5180,.T.);
#5486=ADVANCED_FACE('',(#1081,#591),#762,.T.);
#5487=ADVANCED_FACE('',(#1082,#592),#5181,.F.);
#5488=ADVANCED_FACE('',(#1083),#763,.F.);
#5489=ADVANCED_FACE('',(#1084),#764,.F.);
#5490=ADVANCED_FACE('',(#1085),#765,.F.);
#5491=ADVANCED_FACE('',(#1086),#766,.F.);
#5492=ADVANCED_FACE('',(#1087,#593),#767,.T.);
#5493=ADVANCED_FACE('',(#1088,#594),#5182,.T.);
#5494=ADVANCED_FACE('',(#1089,#595),#768,.T.);
#5495=ADVANCED_FACE('',(#1090,#596),#5183,.F.);
#5496=ADVANCED_FACE('',(#1091),#5184,.F.);
#5497=ADVANCED_FACE('',(#1092),#5185,.F.);
#5498=ADVANCED_FACE('',(#1093),#5186,.F.);
#5499=ADVANCED_FACE('',(#1094),#5187,.F.);
#5500=ADVANCED_FACE('',(#1095),#5188,.F.);
#5501=ADVANCED_FACE('',(#1096),#769,.T.);
#5502=ADVANCED_FACE('',(#1097,#597,#598,#599,#600,#601),#770,.T.);
#5503=ADVANCED_FACE('',(#1098),#771,.T.);
#5504=ADVANCED_FACE('',(#1099,#602,#603,#604,#605,#606),#772,.T.);
#5505=ADVANCED_FACE('',(#1100),#773,.T.);
#5506=ADVANCED_FACE('',(#1101),#774,.F.);
#5507=ADVANCED_FACE('',(#1102),#5189,.F.);
#5508=ADVANCED_FACE('',(#1103),#5190,.T.);
#5509=ADVANCED_FACE('',(#1104,#607),#775,.T.);
#5510=ADVANCED_FACE('',(#1105,#608),#776,.F.);
#5511=ADVANCED_FACE('',(#1106),#5191,.F.);
#5512=ADVANCED_FACE('',(#1107),#5192,.T.);
#5513=ADVANCED_FACE('',(#1108,#609),#777,.T.);
#5514=ADVANCED_FACE('',(#1109,#610),#778,.F.);
#5515=ADVANCED_FACE('',(#1110),#779,.F.);
#5516=ADVANCED_FACE('',(#1111),#780,.F.);
#5517=ADVANCED_FACE('',(#1112),#781,.F.);
#5518=ADVANCED_FACE('',(#1113),#782,.F.);
#5519=ADVANCED_FACE('',(#1114),#783,.F.);
#5520=ADVANCED_FACE('',(#1115),#784,.F.);
#5521=ADVANCED_FACE('',(#1116),#785,.F.);
#5522=ADVANCED_FACE('',(#1117),#786,.F.);
#5523=ADVANCED_FACE('',(#1118),#787,.F.);
#5524=ADVANCED_FACE('',(#1119),#788,.T.);
#5525=ADVANCED_FACE('',(#1120),#327,.T.);
#5526=ADVANCED_FACE('',(#1121),#5193,.T.);
#5527=ADVANCED_FACE('',(#1122),#328,.T.);
#5528=ADVANCED_FACE('',(#1123,#611),#789,.T.);
#5529=ADVANCED_FACE('',(#1124),#329,.T.);
#5530=ADVANCED_FACE('',(#1125),#5194,.T.);
#5531=CLOSED_SHELL('',(#5195,#5196,#5197,#5198,#5199,#5200,#5201,#5202,
#5203,#5204,#5205,#5206,#5207,#5208));
#5532=CLOSED_SHELL('',(#5209,#5210,#5211,#5212,#5213,#5214,#5215,#5216));
#5533=CLOSED_SHELL('',(#5217,#5218,#5219,#5220,#5221,#5222,#5223,#5224));
#5534=CLOSED_SHELL('',(#5225,#5226,#5227,#5228,#5229,#5230,#5231,#5232,
#5233,#5234,#5235,#5236,#5237,#5238,#5239,#5240,#5241,#5242,#5243,#5244,
#5245,#5246,#5247,#5248,#5249,#5250,#5251,#5252,#5253));
#5535=CLOSED_SHELL('',(#5254,#5255,#5256,#5257,#5258,#5259,#5260,#5261,
#5262,#5263,#5264,#5265,#5266,#5267,#5268,#5269,#5270,#5271));
#5536=CLOSED_SHELL('',(#5272,#5273,#5274,#5275,#5276,#5277,#5278,#5279));
#5537=CLOSED_SHELL('',(#5280,#5281,#5282,#5283,#5284,#5285,#5286,#5287));
#5538=CLOSED_SHELL('',(#5288));
#5539=CLOSED_SHELL('',(#5289));
#5540=CLOSED_SHELL('',(#5290));
#5541=CLOSED_SHELL('',(#5291));
#5542=CLOSED_SHELL('',(#5292));
#5543=CLOSED_SHELL('',(#5293));
#5544=CLOSED_SHELL('',(#5294));
#5545=CLOSED_SHELL('',(#5295));
#5546=CLOSED_SHELL('',(#5296,#5297,#5298,#5299,#5300,#5301,#5302,#5303,
#5304,#5305,#5306,#5307,#5308,#5309,#5310,#5311,#5312,#5313,#5314));
#5547=CLOSED_SHELL('',(#5315,#5316,#5317,#5318));
#5548=CLOSED_SHELL('',(#5319,#5320,#5321,#5322));
#5549=CLOSED_SHELL('',(#5323,#5324,#5325,#5326));
#5550=CLOSED_SHELL('',(#5327,#5328,#5329,#5330,#5331,#5332,#5333,#5334,
#5335,#5336,#5337,#5338,#5339,#5340,#5341,#5342));
#5551=CLOSED_SHELL('',(#5343,#5344,#5345,#5346,#5347,#5348,#5349,#5350,
#5351,#5352,#5353,#5354));
#5552=CLOSED_SHELL('',(#5355,#5356,#5357,#5358,#5359,#5360,#5361,#5362,
#5363,#5364,#5365,#5366,#5367,#5368,#5369,#5370,#5371,#5372,#5373,#5374,
#5375));
#5553=CLOSED_SHELL('',(#5376,#5377,#5378,#5379,#5380));
#5554=CLOSED_SHELL('',(#5381,#5382,#5383,#5384));
#5555=CLOSED_SHELL('',(#5385,#5386,#5387,#5388,#5389,#5390,#5391));
#5556=CLOSED_SHELL('',(#5392,#5393,#5394,#5395,#5396,#5397,#5398,#5399,
#5400));
#5557=CLOSED_SHELL('',(#5401,#5402,#5403,#5404,#5405,#5406,#5407,#5408));
#5558=CLOSED_SHELL('',(#5409,#5410,#5411,#5412,#5413,#5414,#5415,#5416,
#5417,#5418,#5419));
#5559=CLOSED_SHELL('',(#5420,#5421,#5422,#5423,#5424,#5425,#5426,#5427,
#5428));
#5560=CLOSED_SHELL('',(#5429,#5430,#5431,#5432));
#5561=CLOSED_SHELL('',(#5433,#5434,#5435,#5436,#5437,#5438,#5439,#5440));
#5562=CLOSED_SHELL('',(#5441,#5442,#5443,#5444));
#5563=CLOSED_SHELL('',(#5445,#5446,#5447,#5448,#5449,#5450,#5451,#5452,
#5453));
#5564=CLOSED_SHELL('',(#5454,#5455,#5456,#5457));
#5565=CLOSED_SHELL('',(#5458,#5459,#5460,#5461,#5462,#5463,#5464,#5465,
#5466,#5467,#5468,#5469,#5470));
#5566=CLOSED_SHELL('',(#5471,#5472,#5473,#5474,#5475,#5476,#5477,#5478,
#5479,#5480,#5481,#5482,#5483,#5484,#5485,#5486,#5487));
#5567=CLOSED_SHELL('',(#5488,#5489,#5490,#5491,#5492,#5493,#5494,#5495));
#5568=CLOSED_SHELL('',(#5496,#5497,#5498,#5499,#5500,#5501,#5502,#5503,
#5504,#5505,#5506));
#5569=CLOSED_SHELL('',(#5507,#5508,#5509,#5510));
#5570=CLOSED_SHELL('',(#5511,#5512,#5513,#5514));
#5571=CLOSED_SHELL('',(#5515,#5516,#5517,#5518,#5519,#5520,#5521,#5522));
#5572=CLOSED_SHELL('',(#5523,#5524,#5525,#5526,#5527,#5528,#5529,#5530));
#5573=DERIVED_UNIT_ELEMENT(#5635,1.);
#5574=DERIVED_UNIT_ELEMENT(#10652,-3.);
#5575=DERIVED_UNIT_ELEMENT(#5635,1.);
#5576=DERIVED_UNIT_ELEMENT(#10652,-3.);
#5577=DERIVED_UNIT_ELEMENT(#5635,1.);
#5578=DERIVED_UNIT_ELEMENT(#10652,-3.);
#5579=DERIVED_UNIT_ELEMENT(#5635,1.);
#5580=DERIVED_UNIT_ELEMENT(#10652,-3.);
#5581=DERIVED_UNIT_ELEMENT(#5635,1.);
#5582=DERIVED_UNIT_ELEMENT(#10652,-3.);
#5583=DERIVED_UNIT_ELEMENT(#5635,1.);
#5584=DERIVED_UNIT_ELEMENT(#10652,-3.);
#5585=DERIVED_UNIT_ELEMENT(#5635,1.);
#5586=DERIVED_UNIT_ELEMENT(#10652,-3.);
#5587=DERIVED_UNIT_ELEMENT(#5635,1.);
#5588=DERIVED_UNIT_ELEMENT(#10652,-3.);
#5589=DERIVED_UNIT_ELEMENT(#5635,1.);
#5590=DERIVED_UNIT_ELEMENT(#10652,-3.);
#5591=DERIVED_UNIT_ELEMENT(#5635,1.);
#5592=DERIVED_UNIT_ELEMENT(#10652,-3.);
#5593=DERIVED_UNIT_ELEMENT(#5635,1.);
#5594=DERIVED_UNIT_ELEMENT(#10652,-3.);
#5595=DERIVED_UNIT_ELEMENT(#5635,1.);
#5596=DERIVED_UNIT_ELEMENT(#10652,-3.);
#5597=DERIVED_UNIT_ELEMENT(#5635,1.);
#5598=DERIVED_UNIT_ELEMENT(#10652,-3.);
#5599=DERIVED_UNIT_ELEMENT(#5635,1.);
#5600=DERIVED_UNIT_ELEMENT(#10652,-3.);
#5601=DERIVED_UNIT_ELEMENT(#5635,1.);
#5602=DERIVED_UNIT_ELEMENT(#10652,-3.);
#5603=DERIVED_UNIT_ELEMENT(#5635,1.);
#5604=DERIVED_UNIT_ELEMENT(#10652,-3.);
#5605=DERIVED_UNIT_ELEMENT(#5635,1.);
#5606=DERIVED_UNIT_ELEMENT(#10652,-3.);
#5607=DERIVED_UNIT_ELEMENT(#5635,1.);
#5608=DERIVED_UNIT_ELEMENT(#10652,-3.);
#5609=DERIVED_UNIT_ELEMENT(#5635,1.);
#5610=DERIVED_UNIT_ELEMENT(#10652,-3.);
#5611=DERIVED_UNIT_ELEMENT(#5635,1.);
#5612=DERIVED_UNIT_ELEMENT(#10652,-3.);
#5613=DERIVED_UNIT_ELEMENT(#5635,1.);
#5614=DERIVED_UNIT_ELEMENT(#10652,-3.);
#5615=DERIVED_UNIT_ELEMENT(#5635,1.);
#5616=DERIVED_UNIT_ELEMENT(#10652,-3.);
#5617=DERIVED_UNIT_ELEMENT(#5635,1.);
#5618=DERIVED_UNIT_ELEMENT(#10652,-3.);
#5619=DERIVED_UNIT_ELEMENT(#5635,1.);
#5620=DERIVED_UNIT_ELEMENT(#10652,-3.);
#5621=DERIVED_UNIT_ELEMENT(#5635,1.);
#5622=DERIVED_UNIT_ELEMENT(#10652,-3.);
#5623=DERIVED_UNIT_ELEMENT(#5635,1.);
#5624=DERIVED_UNIT_ELEMENT(#10652,-3.);
#5625=DERIVED_UNIT_ELEMENT(#5635,1.);
#5626=DERIVED_UNIT_ELEMENT(#10652,-3.);
#5627=DERIVED_UNIT_ELEMENT(#5635,1.);
#5628=DERIVED_UNIT_ELEMENT(#10652,-3.);
#5629=DERIVED_UNIT_ELEMENT(#5635,1.);
#5630=DERIVED_UNIT_ELEMENT(#10652,-3.);
#5631=DERIVED_UNIT_ELEMENT(#5635,1.);
#5632=DERIVED_UNIT_ELEMENT(#10652,-3.);
#5633=DERIVED_UNIT_ELEMENT(#5635,1.);
#5634=DERIVED_UNIT_ELEMENT(#10652,-3.);
#5635=(
MASS_UNIT()
NAMED_UNIT(*)
SI_UNIT(.KILO.,.GRAM.)
);
#5636=DERIVED_UNIT((#5573,#5574));
#5637=DERIVED_UNIT((#5575,#5576));
#5638=DERIVED_UNIT((#5577,#5578));
#5639=DERIVED_UNIT((#5579,#5580));
#5640=DERIVED_UNIT((#5581,#5582));
#5641=DERIVED_UNIT((#5583,#5584));
#5642=DERIVED_UNIT((#5585,#5586));
#5643=DERIVED_UNIT((#5587,#5588));
#5644=DERIVED_UNIT((#5589,#5590));
#5645=DERIVED_UNIT((#5591,#5592));
#5646=DERIVED_UNIT((#5593,#5594));
#5647=DERIVED_UNIT((#5595,#5596));
#5648=DERIVED_UNIT((#5597,#5598));
#5649=DERIVED_UNIT((#5599,#5600));
#5650=DERIVED_UNIT((#5601,#5602));
#5651=DERIVED_UNIT((#5603,#5604));
#5652=DERIVED_UNIT((#5605,#5606));
#5653=DERIVED_UNIT((#5607,#5608));
#5654=DERIVED_UNIT((#5609,#5610));
#5655=DERIVED_UNIT((#5611,#5612));
#5656=DERIVED_UNIT((#5613,#5614));
#5657=DERIVED_UNIT((#5615,#5616));
#5658=DERIVED_UNIT((#5617,#5618));
#5659=DERIVED_UNIT((#5619,#5620));
#5660=DERIVED_UNIT((#5621,#5622));
#5661=DERIVED_UNIT((#5623,#5624));
#5662=DERIVED_UNIT((#5625,#5626));
#5663=DERIVED_UNIT((#5627,#5628));
#5664=DERIVED_UNIT((#5629,#5630));
#5665=DERIVED_UNIT((#5631,#5632));
#5666=DERIVED_UNIT((#5633,#5634));
#5667=MEASURE_REPRESENTATION_ITEM('density measure',
POSITIVE_RATIO_MEASURE(7850.),#5636);
#5668=MEASURE_REPRESENTATION_ITEM('density measure',
POSITIVE_RATIO_MEASURE(7850.),#5637);
#5669=MEASURE_REPRESENTATION_ITEM('density measure',
POSITIVE_RATIO_MEASURE(7850.),#5638);
#5670=MEASURE_REPRESENTATION_ITEM('density measure',
POSITIVE_RATIO_MEASURE(7850.),#5639);
#5671=MEASURE_REPRESENTATION_ITEM('density measure',
POSITIVE_RATIO_MEASURE(7850.),#5640);
#5672=MEASURE_REPRESENTATION_ITEM('density measure',
POSITIVE_RATIO_MEASURE(7850.),#5641);
#5673=MEASURE_REPRESENTATION_ITEM('density measure',
POSITIVE_RATIO_MEASURE(7850.),#5642);
#5674=MEASURE_REPRESENTATION_ITEM('density measure',
POSITIVE_RATIO_MEASURE(7850.),#5643);
#5675=MEASURE_REPRESENTATION_ITEM('density measure',
POSITIVE_RATIO_MEASURE(7850.),#5644);
#5676=MEASURE_REPRESENTATION_ITEM('density measure',
POSITIVE_RATIO_MEASURE(7850.),#5645);
#5677=MEASURE_REPRESENTATION_ITEM('density measure',
POSITIVE_RATIO_MEASURE(7850.),#5646);
#5678=MEASURE_REPRESENTATION_ITEM('density measure',
POSITIVE_RATIO_MEASURE(7850.),#5647);
#5679=MEASURE_REPRESENTATION_ITEM('density measure',
POSITIVE_RATIO_MEASURE(7850.),#5648);
#5680=MEASURE_REPRESENTATION_ITEM('density measure',
POSITIVE_RATIO_MEASURE(7850.),#5649);
#5681=MEASURE_REPRESENTATION_ITEM('density measure',
POSITIVE_RATIO_MEASURE(7850.),#5650);
#5682=MEASURE_REPRESENTATION_ITEM('density measure',
POSITIVE_RATIO_MEASURE(7850.),#5651);
#5683=MEASURE_REPRESENTATION_ITEM('density measure',
POSITIVE_RATIO_MEASURE(7850.),#5652);
#5684=MEASURE_REPRESENTATION_ITEM('density measure',
POSITIVE_RATIO_MEASURE(7850.),#5653);
#5685=MEASURE_REPRESENTATION_ITEM('density measure',
POSITIVE_RATIO_MEASURE(7850.),#5654);
#5686=MEASURE_REPRESENTATION_ITEM('density measure',
POSITIVE_RATIO_MEASURE(7850.),#5655);
#5687=MEASURE_REPRESENTATION_ITEM('density measure',
POSITIVE_RATIO_MEASURE(7850.),#5656);
#5688=MEASURE_REPRESENTATION_ITEM('density measure',
POSITIVE_RATIO_MEASURE(7850.),#5657);
#5689=MEASURE_REPRESENTATION_ITEM('density measure',
POSITIVE_RATIO_MEASURE(7850.),#5658);
#5690=MEASURE_REPRESENTATION_ITEM('density measure',
POSITIVE_RATIO_MEASURE(7850.),#5659);
#5691=MEASURE_REPRESENTATION_ITEM('density measure',
POSITIVE_RATIO_MEASURE(7850.),#5660);
#5692=MEASURE_REPRESENTATION_ITEM('density measure',
POSITIVE_RATIO_MEASURE(7850.),#5661);
#5693=MEASURE_REPRESENTATION_ITEM('density measure',
POSITIVE_RATIO_MEASURE(7850.),#5662);
#5694=MEASURE_REPRESENTATION_ITEM('density measure',
POSITIVE_RATIO_MEASURE(7850.),#5663);
#5695=MEASURE_REPRESENTATION_ITEM('density measure',
POSITIVE_RATIO_MEASURE(7850.),#5664);
#5696=MEASURE_REPRESENTATION_ITEM('density measure',
POSITIVE_RATIO_MEASURE(7850.),#5665);
#5697=MEASURE_REPRESENTATION_ITEM('density measure',
POSITIVE_RATIO_MEASURE(7850.),#5666);
#5698=PROPERTY_DEFINITION_REPRESENTATION(#5853,#5760);
#5699=PROPERTY_DEFINITION_REPRESENTATION(#5854,#5761);
#5700=PROPERTY_DEFINITION_REPRESENTATION(#5855,#5762);
#5701=PROPERTY_DEFINITION_REPRESENTATION(#5856,#5763);
#5702=PROPERTY_DEFINITION_REPRESENTATION(#5857,#5764);
#5703=PROPERTY_DEFINITION_REPRESENTATION(#5858,#5765);
#5704=PROPERTY_DEFINITION_REPRESENTATION(#5859,#5766);
#5705=PROPERTY_DEFINITION_REPRESENTATION(#5860,#5767);
#5706=PROPERTY_DEFINITION_REPRESENTATION(#5861,#5768);
#5707=PROPERTY_DEFINITION_REPRESENTATION(#5862,#5769);
#5708=PROPERTY_DEFINITION_REPRESENTATION(#5863,#5770);
#5709=PROPERTY_DEFINITION_REPRESENTATION(#5864,#5771);
#5710=PROPERTY_DEFINITION_REPRESENTATION(#5865,#5772);
#5711=PROPERTY_DEFINITION_REPRESENTATION(#5866,#5773);
#5712=PROPERTY_DEFINITION_REPRESENTATION(#5867,#5774);
#5713=PROPERTY_DEFINITION_REPRESENTATION(#5868,#5775);
#5714=PROPERTY_DEFINITION_REPRESENTATION(#5869,#5776);
#5715=PROPERTY_DEFINITION_REPRESENTATION(#5870,#5777);
#5716=PROPERTY_DEFINITION_REPRESENTATION(#5871,#5778);
#5717=PROPERTY_DEFINITION_REPRESENTATION(#5872,#5779);
#5718=PROPERTY_DEFINITION_REPRESENTATION(#5873,#5780);
#5719=PROPERTY_DEFINITION_REPRESENTATION(#5874,#5781);
#5720=PROPERTY_DEFINITION_REPRESENTATION(#5875,#5782);
#5721=PROPERTY_DEFINITION_REPRESENTATION(#5876,#5783);
#5722=PROPERTY_DEFINITION_REPRESENTATION(#5877,#5784);
#5723=PROPERTY_DEFINITION_REPRESENTATION(#5878,#5785);
#5724=PROPERTY_DEFINITION_REPRESENTATION(#5879,#5786);
#5725=PROPERTY_DEFINITION_REPRESENTATION(#5880,#5787);
#5726=PROPERTY_DEFINITION_REPRESENTATION(#5881,#5788);
#5727=PROPERTY_DEFINITION_REPRESENTATION(#5882,#5789);
#5728=PROPERTY_DEFINITION_REPRESENTATION(#5883,#5790);
#5729=PROPERTY_DEFINITION_REPRESENTATION(#5884,#5791);
#5730=PROPERTY_DEFINITION_REPRESENTATION(#5885,#5792);
#5731=PROPERTY_DEFINITION_REPRESENTATION(#5886,#5793);
#5732=PROPERTY_DEFINITION_REPRESENTATION(#5887,#5794);
#5733=PROPERTY_DEFINITION_REPRESENTATION(#5888,#5795);
#5734=PROPERTY_DEFINITION_REPRESENTATION(#5889,#5796);
#5735=PROPERTY_DEFINITION_REPRESENTATION(#5890,#5797);
#5736=PROPERTY_DEFINITION_REPRESENTATION(#5891,#5798);
#5737=PROPERTY_DEFINITION_REPRESENTATION(#5892,#5799);
#5738=PROPERTY_DEFINITION_REPRESENTATION(#5893,#5800);
#5739=PROPERTY_DEFINITION_REPRESENTATION(#5894,#5801);
#5740=PROPERTY_DEFINITION_REPRESENTATION(#5895,#5802);
#5741=PROPERTY_DEFINITION_REPRESENTATION(#5896,#5803);
#5742=PROPERTY_DEFINITION_REPRESENTATION(#5897,#5804);
#5743=PROPERTY_DEFINITION_REPRESENTATION(#5898,#5805);
#5744=PROPERTY_DEFINITION_REPRESENTATION(#5899,#5806);
#5745=PROPERTY_DEFINITION_REPRESENTATION(#5900,#5807);
#5746=PROPERTY_DEFINITION_REPRESENTATION(#5901,#5808);
#5747=PROPERTY_DEFINITION_REPRESENTATION(#5902,#5809);
#5748=PROPERTY_DEFINITION_REPRESENTATION(#5903,#5810);
#5749=PROPERTY_DEFINITION_REPRESENTATION(#5904,#5811);
#5750=PROPERTY_DEFINITION_REPRESENTATION(#5905,#5812);
#5751=PROPERTY_DEFINITION_REPRESENTATION(#5906,#5813);
#5752=PROPERTY_DEFINITION_REPRESENTATION(#5907,#5814);
#5753=PROPERTY_DEFINITION_REPRESENTATION(#5908,#5815);
#5754=PROPERTY_DEFINITION_REPRESENTATION(#5909,#5816);
#5755=PROPERTY_DEFINITION_REPRESENTATION(#5910,#5817);
#5756=PROPERTY_DEFINITION_REPRESENTATION(#5911,#5818);
#5757=PROPERTY_DEFINITION_REPRESENTATION(#5912,#5819);
#5758=PROPERTY_DEFINITION_REPRESENTATION(#5913,#5820);
#5759=PROPERTY_DEFINITION_REPRESENTATION(#5914,#5821);
#5760=REPRESENTATION('material name',(#5822),#10614);
#5761=REPRESENTATION('density',(#5667),#10614);
#5762=REPRESENTATION('material name',(#5823),#10615);
#5763=REPRESENTATION('density',(#5668),#10615);
#5764=REPRESENTATION('material name',(#5824),#10616);
#5765=REPRESENTATION('density',(#5669),#10616);
#5766=REPRESENTATION('material name',(#5825),#10617);
#5767=REPRESENTATION('density',(#5670),#10617);
#5768=REPRESENTATION('material name',(#5826),#10619);
#5769=REPRESENTATION('density',(#5671),#10619);
#5770=REPRESENTATION('material name',(#5827),#10620);
#5771=REPRESENTATION('density',(#5672),#10620);
#5772=REPRESENTATION('material name',(#5828),#10621);
#5773=REPRESENTATION('density',(#5673),#10621);
#5774=REPRESENTATION('material name',(#5829),#10622);
#5775=REPRESENTATION('density',(#5674),#10622);
#5776=REPRESENTATION('material name',(#5830),#10623);
#5777=REPRESENTATION('density',(#5675),#10623);
#5778=REPRESENTATION('material name',(#5831),#10624);
#5779=REPRESENTATION('density',(#5676),#10624);
#5780=REPRESENTATION('material name',(#5832),#10625);
#5781=REPRESENTATION('density',(#5677),#10625);
#5782=REPRESENTATION('material name',(#5833),#10626);
#5783=REPRESENTATION('density',(#5678),#10626);
#5784=REPRESENTATION('material name',(#5834),#10628);
#5785=REPRESENTATION('density',(#5679),#10628);
#5786=REPRESENTATION('material name',(#5835),#10629);
#5787=REPRESENTATION('density',(#5680),#10629);
#5788=REPRESENTATION('material name',(#5836),#10630);
#5789=REPRESENTATION('density',(#5681),#10630);
#5790=REPRESENTATION('material name',(#5837),#10631);
#5791=REPRESENTATION('density',(#5682),#10631);
#5792=REPRESENTATION('material name',(#5838),#10632);
#5793=REPRESENTATION('density',(#5683),#10632);
#5794=REPRESENTATION('material name',(#5839),#10633);
#5795=REPRESENTATION('density',(#5684),#10633);
#5796=REPRESENTATION('material name',(#5840),#10634);
#5797=REPRESENTATION('density',(#5685),#10634);
#5798=REPRESENTATION('material name',(#5841),#10635);
#5799=REPRESENTATION('density',(#5686),#10635);
#5800=REPRESENTATION('material name',(#5842),#10637);
#5801=REPRESENTATION('density',(#5687),#10637);
#5802=REPRESENTATION('material name',(#5843),#10638);
#5803=REPRESENTATION('density',(#5688),#10638);
#5804=REPRESENTATION('material name',(#5844),#10640);
#5805=REPRESENTATION('density',(#5689),#10640);
#5806=REPRESENTATION('material name',(#5845),#10641);
#5807=REPRESENTATION('density',(#5690),#10641);
#5808=REPRESENTATION('material name',(#5846),#10642);
#5809=REPRESENTATION('density',(#5691),#10642);
#5810=REPRESENTATION('material name',(#5847),#10644);
#5811=REPRESENTATION('density',(#5692),#10644);
#5812=REPRESENTATION('material name',(#5848),#10645);
#5813=REPRESENTATION('density',(#5693),#10645);
#5814=REPRESENTATION('material name',(#5849),#10646);
#5815=REPRESENTATION('density',(#5694),#10646);
#5816=REPRESENTATION('material name',(#5850),#10647);
#5817=REPRESENTATION('density',(#5695),#10647);
#5818=REPRESENTATION('material name',(#5851),#10648);
#5819=REPRESENTATION('density',(#5696),#10648);
#5820=REPRESENTATION('material name',(#5852),#10649);
#5821=REPRESENTATION('density',(#5697),#10649);
#5822=DESCRIPTIVE_REPRESENTATION_ITEM('Steel','Steel');
#5823=DESCRIPTIVE_REPRESENTATION_ITEM('Steel','Steel');
#5824=DESCRIPTIVE_REPRESENTATION_ITEM('Steel','Steel');
#5825=DESCRIPTIVE_REPRESENTATION_ITEM('Steel','Steel');
#5826=DESCRIPTIVE_REPRESENTATION_ITEM('Steel','Steel');
#5827=DESCRIPTIVE_REPRESENTATION_ITEM('Steel','Steel');
#5828=DESCRIPTIVE_REPRESENTATION_ITEM('Steel','Steel');
#5829=DESCRIPTIVE_REPRESENTATION_ITEM('Steel','Steel');
#5830=DESCRIPTIVE_REPRESENTATION_ITEM('Steel','Steel');
#5831=DESCRIPTIVE_REPRESENTATION_ITEM('Steel','Steel');
#5832=DESCRIPTIVE_REPRESENTATION_ITEM('Steel','Steel');
#5833=DESCRIPTIVE_REPRESENTATION_ITEM('Steel','Steel');
#5834=DESCRIPTIVE_REPRESENTATION_ITEM('Steel','Steel');
#5835=DESCRIPTIVE_REPRESENTATION_ITEM('Steel','Steel');
#5836=DESCRIPTIVE_REPRESENTATION_ITEM('Steel','Steel');
#5837=DESCRIPTIVE_REPRESENTATION_ITEM('Steel','Steel');
#5838=DESCRIPTIVE_REPRESENTATION_ITEM('Steel','Steel');
#5839=DESCRIPTIVE_REPRESENTATION_ITEM('Steel','Steel');
#5840=DESCRIPTIVE_REPRESENTATION_ITEM('Steel','Steel');
#5841=DESCRIPTIVE_REPRESENTATION_ITEM('Steel','Steel');
#5842=DESCRIPTIVE_REPRESENTATION_ITEM('Steel','Steel');
#5843=DESCRIPTIVE_REPRESENTATION_ITEM('Steel','Steel');
#5844=DESCRIPTIVE_REPRESENTATION_ITEM('Steel','Steel');
#5845=DESCRIPTIVE_REPRESENTATION_ITEM('Steel','Steel');
#5846=DESCRIPTIVE_REPRESENTATION_ITEM('Steel','Steel');
#5847=DESCRIPTIVE_REPRESENTATION_ITEM('Steel','Steel');
#5848=DESCRIPTIVE_REPRESENTATION_ITEM('Steel','Steel');
#5849=DESCRIPTIVE_REPRESENTATION_ITEM('Steel','Steel');
#5850=DESCRIPTIVE_REPRESENTATION_ITEM('Steel','Steel');
#5851=DESCRIPTIVE_REPRESENTATION_ITEM('Steel','Steel');
#5852=DESCRIPTIVE_REPRESENTATION_ITEM('Steel','Steel');
#5853=PROPERTY_DEFINITION('material property','material name',#10835);
#5854=PROPERTY_DEFINITION('material property','density of part',#10835);
#5855=PROPERTY_DEFINITION('material property','material name',#10836);
#5856=PROPERTY_DEFINITION('material property','density of part',#10836);
#5857=PROPERTY_DEFINITION('material property','material name',#10837);
#5858=PROPERTY_DEFINITION('material property','density of part',#10837);
#5859=PROPERTY_DEFINITION('material property','material name',#10838);
#5860=PROPERTY_DEFINITION('material property','density of part',#10838);
#5861=PROPERTY_DEFINITION('material property','material name',#10840);
#5862=PROPERTY_DEFINITION('material property','density of part',#10840);
#5863=PROPERTY_DEFINITION('material property','material name',#10841);
#5864=PROPERTY_DEFINITION('material property','density of part',#10841);
#5865=PROPERTY_DEFINITION('material property','material name',#10842);
#5866=PROPERTY_DEFINITION('material property','density of part',#10842);
#5867=PROPERTY_DEFINITION('material property','material name',#10843);
#5868=PROPERTY_DEFINITION('material property','density of part',#10843);
#5869=PROPERTY_DEFINITION('material property','material name',#10844);
#5870=PROPERTY_DEFINITION('material property','density of part',#10844);
#5871=PROPERTY_DEFINITION('material property','material name',#10845);
#5872=PROPERTY_DEFINITION('material property','density of part',#10845);
#5873=PROPERTY_DEFINITION('material property','material name',#10846);
#5874=PROPERTY_DEFINITION('material property','density of part',#10846);
#5875=PROPERTY_DEFINITION('material property','material name',#10847);
#5876=PROPERTY_DEFINITION('material property','density of part',#10847);
#5877=PROPERTY_DEFINITION('material property','material name',#10849);
#5878=PROPERTY_DEFINITION('material property','density of part',#10849);
#5879=PROPERTY_DEFINITION('material property','material name',#10850);
#5880=PROPERTY_DEFINITION('material property','density of part',#10850);
#5881=PROPERTY_DEFINITION('material property','material name',#10851);
#5882=PROPERTY_DEFINITION('material property','density of part',#10851);
#5883=PROPERTY_DEFINITION('material property','material name',#10852);
#5884=PROPERTY_DEFINITION('material property','density of part',#10852);
#5885=PROPERTY_DEFINITION('material property','material name',#10853);
#5886=PROPERTY_DEFINITION('material property','density of part',#10853);
#5887=PROPERTY_DEFINITION('material property','material name',#10854);
#5888=PROPERTY_DEFINITION('material property','density of part',#10854);
#5889=PROPERTY_DEFINITION('material property','material name',#10855);
#5890=PROPERTY_DEFINITION('material property','density of part',#10855);
#5891=PROPERTY_DEFINITION('material property','material name',#10856);
#5892=PROPERTY_DEFINITION('material property','density of part',#10856);
#5893=PROPERTY_DEFINITION('material property','material name',#10858);
#5894=PROPERTY_DEFINITION('material property','density of part',#10858);
#5895=PROPERTY_DEFINITION('material property','material name',#10859);
#5896=PROPERTY_DEFINITION('material property','density of part',#10859);
#5897=PROPERTY_DEFINITION('material property','material name',#10861);
#5898=PROPERTY_DEFINITION('material property','density of part',#10861);
#5899=PROPERTY_DEFINITION('material property','material name',#10862);
#5900=PROPERTY_DEFINITION('material property','density of part',#10862);
#5901=PROPERTY_DEFINITION('material property','material name',#10863);
#5902=PROPERTY_DEFINITION('material property','density of part',#10863);
#5903=PROPERTY_DEFINITION('material property','material name',#10865);
#5904=PROPERTY_DEFINITION('material property','density of part',#10865);
#5905=PROPERTY_DEFINITION('material property','material name',#10866);
#5906=PROPERTY_DEFINITION('material property','density of part',#10866);
#5907=PROPERTY_DEFINITION('material property','material name',#10867);
#5908=PROPERTY_DEFINITION('material property','density of part',#10867);
#5909=PROPERTY_DEFINITION('material property','material name',#10868);
#5910=PROPERTY_DEFINITION('material property','density of part',#10868);
#5911=PROPERTY_DEFINITION('material property','material name',#10869);
#5912=PROPERTY_DEFINITION('material property','density of part',#10869);
#5913=PROPERTY_DEFINITION('material property','material name',#10870);
#5914=PROPERTY_DEFINITION('material property','density of part',#10870);
#5915=AXIS2_PLACEMENT_3D('',#8512,#6671,#6672);
#5916=AXIS2_PLACEMENT_3D('',#8513,#6673,#6674);
#5917=AXIS2_PLACEMENT_3D('',#8514,#6675,#6676);
#5918=AXIS2_PLACEMENT_3D('',#8515,#6677,#6678);
#5919=AXIS2_PLACEMENT_3D('',#8517,#6679,#6680);
#5920=AXIS2_PLACEMENT_3D('',#8520,#6682,#6683);
#5921=AXIS2_PLACEMENT_3D('',#8521,#6684,#6685);
#5922=AXIS2_PLACEMENT_3D('',#8523,#6686,#6687);
#5923=AXIS2_PLACEMENT_3D('',#8526,#6689,#6690);
#5924=AXIS2_PLACEMENT_3D('',#8527,#6691,#6692);
#5925=AXIS2_PLACEMENT_3D('',#8529,#6693,#6694);
#5926=AXIS2_PLACEMENT_3D('',#8532,#6696,#6697);
#5927=AXIS2_PLACEMENT_3D('',#8533,#6698,#6699);
#5928=AXIS2_PLACEMENT_3D('',#8535,#6700,#6701);
#5929=AXIS2_PLACEMENT_3D('',#8538,#6703,#6704);
#5930=AXIS2_PLACEMENT_3D('',#8539,#6705,#6706);
#5931=AXIS2_PLACEMENT_3D('',#8541,#6707,#6708);
#5932=AXIS2_PLACEMENT_3D('',#8544,#6710,#6711);
#5933=AXIS2_PLACEMENT_3D('',#8545,#6712,#6713);
#5934=AXIS2_PLACEMENT_3D('',#8547,#6714,#6715);
#5935=AXIS2_PLACEMENT_3D('',#8550,#6717,#6718);
#5936=AXIS2_PLACEMENT_3D('',#8551,#6719,#6720);
#5937=AXIS2_PLACEMENT_3D('',#8553,#6721,#6722);
#5938=AXIS2_PLACEMENT_3D('',#8556,#6724,#6725);
#5939=AXIS2_PLACEMENT_3D('',#8557,#6726,#6727);
#5940=AXIS2_PLACEMENT_3D('',#8559,#6728,#6729);
#5941=AXIS2_PLACEMENT_3D('',#8562,#6731,#6732);
#5942=AXIS2_PLACEMENT_3D('',#8563,#6733,#6734);
#5943=AXIS2_PLACEMENT_3D('',#8572,#6739,#6740);
#5944=AXIS2_PLACEMENT_3D('',#8578,#6744,#6745);
#5945=AXIS2_PLACEMENT_3D('',#8584,#6749,#6750);
#5946=AXIS2_PLACEMENT_3D('',#8587,#6753,#6754);
#5947=AXIS2_PLACEMENT_3D('',#8588,#6755,#6756);
#5948=AXIS2_PLACEMENT_3D('',#8589,#6757,#6758);
#5949=AXIS2_PLACEMENT_3D('',#8590,#6759,#6760);
#5950=AXIS2_PLACEMENT_3D('',#8599,#6765,#6766);
#5951=AXIS2_PLACEMENT_3D('',#8605,#6770,#6771);
#5952=AXIS2_PLACEMENT_3D('',#8611,#6775,#6776);
#5953=AXIS2_PLACEMENT_3D('',#8617,#6780,#6781);
#5954=AXIS2_PLACEMENT_3D('',#8623,#6785,#6786);
#5955=AXIS2_PLACEMENT_3D('',#8626,#6789,#6790);
#5956=AXIS2_PLACEMENT_3D('',#8627,#6791,#6792);
#5957=AXIS2_PLACEMENT_3D('',#8628,#6793,#6794);
#5958=AXIS2_PLACEMENT_3D('',#8630,#6795,#6796);
#5959=AXIS2_PLACEMENT_3D('',#8631,#6797,#6798);
#5960=AXIS2_PLACEMENT_3D('',#8633,#6799,#6800);
#5961=AXIS2_PLACEMENT_3D('',#8634,#6801,#6802);
#5962=AXIS2_PLACEMENT_3D('',#8636,#6803,#6804);
#5963=AXIS2_PLACEMENT_3D('',#8638,#6806,#6807);
#5964=AXIS2_PLACEMENT_3D('',#8640,#6808,#6809);
#5965=AXIS2_PLACEMENT_3D('',#8642,#6811,#6812);
#5966=AXIS2_PLACEMENT_3D('',#8644,#6813,#6814);
#5967=AXIS2_PLACEMENT_3D('',#8646,#6816,#6817);
#5968=AXIS2_PLACEMENT_3D('',#8648,#6818,#6819);
#5969=AXIS2_PLACEMENT_3D('',#8649,#6820,#6821);
#5970=AXIS2_PLACEMENT_3D('',#8651,#6822,#6823);
#5971=AXIS2_PLACEMENT_3D('',#8653,#6825,#6826);
#5972=AXIS2_PLACEMENT_3D('',#8655,#6828,#6829);
#5973=AXIS2_PLACEMENT_3D('',#8656,#6830,#6831);
#5974=AXIS2_PLACEMENT_3D('',#8734,#6833,#6834);
#5975=AXIS2_PLACEMENT_3D('',#8736,#6835,#6836);
#5976=AXIS2_PLACEMENT_3D('',#8739,#6838,#6839);
#5977=AXIS2_PLACEMENT_3D('',#8740,#6840,#6841);
#5978=AXIS2_PLACEMENT_3D('',#8741,#6842,#6843);
#5979=AXIS2_PLACEMENT_3D('',#8743,#6844,#6845);
#5980=AXIS2_PLACEMENT_3D('',#8746,#6847,#6848);
#5981=AXIS2_PLACEMENT_3D('',#8747,#6849,#6850);
#5982=AXIS2_PLACEMENT_3D('',#8748,#6851,#6852);
#5983=AXIS2_PLACEMENT_3D('',#8750,#6853,#6854);
#5984=AXIS2_PLACEMENT_3D('',#8753,#6856,#6857);
#5985=AXIS2_PLACEMENT_3D('',#8754,#6858,#6859);
#5986=AXIS2_PLACEMENT_3D('',#8755,#6860,#6861);
#5987=AXIS2_PLACEMENT_3D('',#8757,#6862,#6863);
#5988=AXIS2_PLACEMENT_3D('',#8760,#6865,#6866);
#5989=AXIS2_PLACEMENT_3D('',#8761,#6867,#6868);
#5990=AXIS2_PLACEMENT_3D('',#8762,#6869,#6870);
#5991=AXIS2_PLACEMENT_3D('',#8765,#6871,#6872);
#5992=AXIS2_PLACEMENT_3D('',#8766,#6873,#6874);
#5993=AXIS2_PLACEMENT_3D('',#8767,#6875,#6876);
#5994=AXIS2_PLACEMENT_3D('',#8771,#6878,#6879);
#5995=AXIS2_PLACEMENT_3D('',#8773,#6881,#6882);
#5996=AXIS2_PLACEMENT_3D('',#8778,#6884,#6885);
#5997=AXIS2_PLACEMENT_3D('',#8781,#6887,#6888);
#5998=AXIS2_PLACEMENT_3D('',#8782,#6889,#6890);
#5999=AXIS2_PLACEMENT_3D('',#8783,#6891,#6892);
#6000=AXIS2_PLACEMENT_3D('',#8784,#6893,#6894);
#6001=AXIS2_PLACEMENT_3D('',#8789,#6896,#6897);
#6002=AXIS2_PLACEMENT_3D('',#8792,#6899,#6900);
#6003=AXIS2_PLACEMENT_3D('',#8793,#6901,#6902);
#6004=AXIS2_PLACEMENT_3D('',#8794,#6903,#6904);
#6005=AXIS2_PLACEMENT_3D('',#8795,#6905,#6906);
#6006=AXIS2_PLACEMENT_3D('',#8800,#6908,#6909);
#6007=AXIS2_PLACEMENT_3D('',#8803,#6911,#6912);
#6008=AXIS2_PLACEMENT_3D('',#8804,#6913,#6914);
#6009=AXIS2_PLACEMENT_3D('',#8805,#6915,#6916);
#6010=AXIS2_PLACEMENT_3D('',#8806,#6917,#6918);
#6011=AXIS2_PLACEMENT_3D('',#8808,#6919,#6920);
#6012=AXIS2_PLACEMENT_3D('',#8811,#6922,#6923);
#6013=AXIS2_PLACEMENT_3D('',#8812,#6924,#6925);
#6014=AXIS2_PLACEMENT_3D('',#8813,#6926,#6927);
#6015=AXIS2_PLACEMENT_3D('',#8814,#6928,#6929);
#6016=AXIS2_PLACEMENT_3D('',#8815,#6930,#6931);
#6017=AXIS2_PLACEMENT_3D('',#8816,#6932,#6933);
#6018=AXIS2_PLACEMENT_3D('',#8818,#6934,#6935);
#6019=AXIS2_PLACEMENT_3D('',#8820,#6936,#6937);
#6020=AXIS2_PLACEMENT_3D('',#8822,#6938,#6939);
#6021=AXIS2_PLACEMENT_3D('',#8824,#6940,#6941);
#6022=AXIS2_PLACEMENT_3D('',#8826,#6942,#6943);
#6023=AXIS2_PLACEMENT_3D('',#8827,#6944,#6945);
#6024=AXIS2_PLACEMENT_3D('',#8829,#6946,#6947);
#6025=AXIS2_PLACEMENT_3D('',#8831,#6949,#6950);
#6026=AXIS2_PLACEMENT_3D('',#8833,#6951,#6952);
#6027=AXIS2_PLACEMENT_3D('',#8835,#6954,#6955);
#6028=AXIS2_PLACEMENT_3D('',#8837,#6956,#6957);
#6029=AXIS2_PLACEMENT_3D('',#8839,#6959,#6960);
#6030=AXIS2_PLACEMENT_3D('',#8841,#6961,#6962);
#6031=AXIS2_PLACEMENT_3D('',#8843,#6964,#6965);
#6032=AXIS2_PLACEMENT_3D('',#8845,#6966,#6967);
#6033=AXIS2_PLACEMENT_3D('',#8848,#6969,#6970);
#6034=AXIS2_PLACEMENT_3D('',#8849,#6971,#6972);
#6035=AXIS2_PLACEMENT_3D('',#8851,#6973,#6974);
#6036=AXIS2_PLACEMENT_3D('',#8852,#6975,#6976);
#6037=AXIS2_PLACEMENT_3D('',#8855,#6978,#6979);
#6038=AXIS2_PLACEMENT_3D('',#8856,#6980,#6981);
#6039=AXIS2_PLACEMENT_3D('',#8859,#6983,#6984);
#6040=AXIS2_PLACEMENT_3D('',#8860,#6985,#6986);
#6041=AXIS2_PLACEMENT_3D('',#8861,#6987,#6988);
#6042=AXIS2_PLACEMENT_3D('',#8862,#6989,#6990);
#6043=AXIS2_PLACEMENT_3D('',#8863,#6991,#6992);
#6044=AXIS2_PLACEMENT_3D('',#8865,#6993,#6994);
#6045=AXIS2_PLACEMENT_3D('',#8868,#6996,#6997);
#6046=AXIS2_PLACEMENT_3D('',#8869,#6998,#6999);
#6047=AXIS2_PLACEMENT_3D('',#8871,#7000,#7001);
#6048=AXIS2_PLACEMENT_3D('',#8872,#7002,#7003);
#6049=AXIS2_PLACEMENT_3D('',#8874,#7004,#7005);
#6050=AXIS2_PLACEMENT_3D('',#8877,#7007,#7008);
#6051=AXIS2_PLACEMENT_3D('',#8878,#7009,#7010);
#6052=AXIS2_PLACEMENT_3D('',#8880,#7011,#7012);
#6053=AXIS2_PLACEMENT_3D('',#8881,#7013,#7014);
#6054=AXIS2_PLACEMENT_3D('',#8883,#7015,#7016);
#6055=AXIS2_PLACEMENT_3D('',#8886,#7018,#7019);
#6056=AXIS2_PLACEMENT_3D('',#8887,#7020,#7021);
#6057=AXIS2_PLACEMENT_3D('',#8889,#7022,#7023);
#6058=AXIS2_PLACEMENT_3D('',#8890,#7024,#7025);
#6059=AXIS2_PLACEMENT_3D('',#8892,#7026,#7027);
#6060=AXIS2_PLACEMENT_3D('',#8895,#7029,#7030);
#6061=AXIS2_PLACEMENT_3D('',#8896,#7031,#7032);
#6062=AXIS2_PLACEMENT_3D('',#8898,#7033,#7034);
#6063=AXIS2_PLACEMENT_3D('',#8899,#7035,#7036);
#6064=AXIS2_PLACEMENT_3D('',#8901,#7037,#7038);
#6065=AXIS2_PLACEMENT_3D('',#8903,#7040,#7041);
#6066=AXIS2_PLACEMENT_3D('',#8905,#7042,#7043);
#6067=AXIS2_PLACEMENT_3D('',#8907,#7045,#7046);
#6068=AXIS2_PLACEMENT_3D('',#8909,#7047,#7048);
#6069=AXIS2_PLACEMENT_3D('',#8911,#7050,#7051);
#6070=AXIS2_PLACEMENT_3D('',#8913,#7052,#7053);
#6071=AXIS2_PLACEMENT_3D('',#8915,#7055,#7056);
#6072=AXIS2_PLACEMENT_3D('',#8917,#7057,#7058);
#6073=AXIS2_PLACEMENT_3D('',#8920,#7060,#7061);
#6074=AXIS2_PLACEMENT_3D('',#8921,#7062,#7063);
#6075=AXIS2_PLACEMENT_3D('',#8923,#7064,#7065);
#6076=AXIS2_PLACEMENT_3D('',#8924,#7066,#7067);
#6077=AXIS2_PLACEMENT_3D('',#8926,#7068,#7069);
#6078=AXIS2_PLACEMENT_3D('',#8928,#7071,#7072);
#6079=AXIS2_PLACEMENT_3D('',#8930,#7073,#7074);
#6080=AXIS2_PLACEMENT_3D('',#8933,#7076,#7077);
#6081=AXIS2_PLACEMENT_3D('',#8934,#7078,#7079);
#6082=AXIS2_PLACEMENT_3D('',#8935,#7080,#7081);
#6083=AXIS2_PLACEMENT_3D('',#8936,#7082,#7083);
#6084=AXIS2_PLACEMENT_3D('',#8937,#7084,#7085);
#6085=AXIS2_PLACEMENT_3D('',#8938,#7086,#7087);
#6086=AXIS2_PLACEMENT_3D('',#8941,#7088,#7089);
#6087=AXIS2_PLACEMENT_3D('',#8942,#7090,#7091);
#6088=AXIS2_PLACEMENT_3D('',#8944,#7092,#7093);
#6089=AXIS2_PLACEMENT_3D('',#8946,#7094,#7095);
#6090=AXIS2_PLACEMENT_3D('',#8947,#7096,#7097);
#6091=AXIS2_PLACEMENT_3D('',#8948,#7098,#7099);
#6092=AXIS2_PLACEMENT_3D('',#8951,#7101,#7102);
#6093=AXIS2_PLACEMENT_3D('',#8952,#7103,#7104);
#6094=AXIS2_PLACEMENT_3D('',#8954,#7105,#7106);
#6095=AXIS2_PLACEMENT_3D('',#8957,#7108,#7109);
#6096=AXIS2_PLACEMENT_3D('',#8958,#7110,#7111);
#6097=AXIS2_PLACEMENT_3D('',#8961,#7113,#7114);
#6098=AXIS2_PLACEMENT_3D('',#8962,#7115,#7116);
#6099=AXIS2_PLACEMENT_3D('',#8963,#7117,#7118);
#6100=AXIS2_PLACEMENT_3D('',#8965,#7119,#7120);
#6101=AXIS2_PLACEMENT_3D('',#8967,#7122,#7123);
#6102=AXIS2_PLACEMENT_3D('',#8969,#7124,#7125);
#6103=AXIS2_PLACEMENT_3D('',#8970,#7126,#7127);
#6104=AXIS2_PLACEMENT_3D('',#8972,#7129,#7130);
#6105=AXIS2_PLACEMENT_3D('',#8973,#7131,#7132);
#6106=AXIS2_PLACEMENT_3D('',#8976,#7133,#7134);
#6107=AXIS2_PLACEMENT_3D('',#8977,#7135,#7136);
#6108=AXIS2_PLACEMENT_3D('',#8979,#7137,#7138);
#6109=AXIS2_PLACEMENT_3D('',#8981,#7139,#7140);
#6110=AXIS2_PLACEMENT_3D('',#8982,#7141,#7142);
#6111=AXIS2_PLACEMENT_3D('',#8983,#7143,#7144);
#6112=AXIS2_PLACEMENT_3D('',#8985,#7145,#7146);
#6113=AXIS2_PLACEMENT_3D('',#8987,#7148,#7149);
#6114=AXIS2_PLACEMENT_3D('',#8989,#7150,#7151);
#6115=AXIS2_PLACEMENT_3D('',#8991,#7152,#7153);
#6116=AXIS2_PLACEMENT_3D('',#8992,#7154,#7155);
#6117=AXIS2_PLACEMENT_3D('',#8994,#7156,#7157);
#6118=AXIS2_PLACEMENT_3D('',#8996,#7159,#7160);
#6119=AXIS2_PLACEMENT_3D('',#8998,#7161,#7162);
#6120=AXIS2_PLACEMENT_3D('',#9000,#7164,#7165);
#6121=AXIS2_PLACEMENT_3D('',#9002,#7166,#7167);
#6122=AXIS2_PLACEMENT_3D('',#9004,#7169,#7170);
#6123=AXIS2_PLACEMENT_3D('',#9005,#7171,#7172);
#6124=AXIS2_PLACEMENT_3D('',#9007,#7174,#7175);
#6125=AXIS2_PLACEMENT_3D('',#9008,#7176,#7177);
#6126=AXIS2_PLACEMENT_3D('',#9011,#7178,#7179);
#6127=AXIS2_PLACEMENT_3D('',#9012,#7180,#7181);
#6128=AXIS2_PLACEMENT_3D('',#9015,#7182,#7183);
#6129=AXIS2_PLACEMENT_3D('',#9016,#7184,#7185);
#6130=AXIS2_PLACEMENT_3D('',#9019,#7186,#7187);
#6131=AXIS2_PLACEMENT_3D('',#9020,#7188,#7189);
#6132=AXIS2_PLACEMENT_3D('',#9023,#7190,#7191);
#6133=AXIS2_PLACEMENT_3D('',#9024,#7192,#7193);
#6134=AXIS2_PLACEMENT_3D('',#9027,#7194,#7195);
#6135=AXIS2_PLACEMENT_3D('',#9028,#7196,#7197);
#6136=AXIS2_PLACEMENT_3D('',#9031,#7198,#7199);
#6137=AXIS2_PLACEMENT_3D('',#9032,#7200,#7201);
#6138=AXIS2_PLACEMENT_3D('',#9035,#7202,#7203);
#6139=AXIS2_PLACEMENT_3D('',#9036,#7204,#7205);
#6140=AXIS2_PLACEMENT_3D('',#9039,#7206,#7207);
#6141=AXIS2_PLACEMENT_3D('',#9040,#7208,#7209);
#6142=AXIS2_PLACEMENT_3D('',#9041,#7210,#7211);
#6143=AXIS2_PLACEMENT_3D('',#9067,#7212,#7213);
#6144=AXIS2_PLACEMENT_3D('',#9091,#7214,#7215);
#6145=AXIS2_PLACEMENT_3D('',#9092,#7216,#7217);
#6146=AXIS2_PLACEMENT_3D('',#9094,#7218,#7219);
#6147=AXIS2_PLACEMENT_3D('',#9119,#7220,#7221);
#6148=AXIS2_PLACEMENT_3D('',#9144,#7222,#7223);
#6149=AXIS2_PLACEMENT_3D('',#9160,#7225,#7226);
#6150=AXIS2_PLACEMENT_3D('',#9175,#7227,#7228);
#6151=AXIS2_PLACEMENT_3D('',#9200,#7229,#7230);
#6152=AXIS2_PLACEMENT_3D('',#9225,#7231,#7232);
#6153=AXIS2_PLACEMENT_3D('',#9250,#7233,#7234);
#6154=AXIS2_PLACEMENT_3D('',#9274,#7235,#7236);
#6155=AXIS2_PLACEMENT_3D('',#9275,#7237,#7238);
#6156=AXIS2_PLACEMENT_3D('',#9277,#7239,#7240);
#6157=AXIS2_PLACEMENT_3D('',#9278,#7241,#7242);
#6158=AXIS2_PLACEMENT_3D('',#9279,#7243,#7244);
#6159=AXIS2_PLACEMENT_3D('',#9303,#7245,#7246);
#6160=AXIS2_PLACEMENT_3D('',#9304,#7247,#7248);
#6161=AXIS2_PLACEMENT_3D('',#9306,#7249,#7250);
#6162=AXIS2_PLACEMENT_3D('',#9307,#7251,#7252);
#6163=AXIS2_PLACEMENT_3D('',#9308,#7253,#7254);
#6164=AXIS2_PLACEMENT_3D('',#9332,#7255,#7256);
#6165=AXIS2_PLACEMENT_3D('',#9333,#7257,#7258);
#6166=AXIS2_PLACEMENT_3D('',#9335,#7259,#7260);
#6167=AXIS2_PLACEMENT_3D('',#9336,#7261,#7262);
#6168=AXIS2_PLACEMENT_3D('',#9337,#7263,#7264);
#6169=AXIS2_PLACEMENT_3D('',#9352,#7265,#7266);
#6170=AXIS2_PLACEMENT_3D('',#9365,#7267,#7268);
#6171=AXIS2_PLACEMENT_3D('',#9367,#7269,#7270);
#6172=AXIS2_PLACEMENT_3D('',#9368,#7271,#7272);
#6173=AXIS2_PLACEMENT_3D('',#9369,#7273,#7274);
#6174=AXIS2_PLACEMENT_3D('',#9393,#7275,#7276);
#6175=AXIS2_PLACEMENT_3D('',#9394,#7277,#7278);
#6176=AXIS2_PLACEMENT_3D('',#9396,#7279,#7280);
#6177=AXIS2_PLACEMENT_3D('',#9397,#7281,#7282);
#6178=AXIS2_PLACEMENT_3D('',#9398,#7283,#7284);
#6179=AXIS2_PLACEMENT_3D('',#9422,#7285,#7286);
#6180=AXIS2_PLACEMENT_3D('',#9423,#7287,#7288);
#6181=AXIS2_PLACEMENT_3D('',#9425,#7289,#7290);
#6182=AXIS2_PLACEMENT_3D('',#9426,#7291,#7292);
#6183=AXIS2_PLACEMENT_3D('',#9427,#7293,#7294);
#6184=AXIS2_PLACEMENT_3D('',#9451,#7295,#7296);
#6185=AXIS2_PLACEMENT_3D('',#9452,#7297,#7298);
#6186=AXIS2_PLACEMENT_3D('',#9454,#7299,#7300);
#6187=AXIS2_PLACEMENT_3D('',#9457,#7302,#7303);
#6188=AXIS2_PLACEMENT_3D('',#9481,#7304,#7305);
#6189=AXIS2_PLACEMENT_3D('',#9482,#7306,#7307);
#6190=AXIS2_PLACEMENT_3D('',#9483,#7308,#7309);
#6191=AXIS2_PLACEMENT_3D('',#9484,#7310,#7311);
#6192=AXIS2_PLACEMENT_3D('',#9485,#7312,#7313);
#6193=AXIS2_PLACEMENT_3D('',#9486,#7314,#7315);
#6194=AXIS2_PLACEMENT_3D('',#9487,#7316,#7317);
#6195=AXIS2_PLACEMENT_3D('',#9488,#7318,#7319);
#6196=AXIS2_PLACEMENT_3D('',#9489,#7320,#7321);
#6197=AXIS2_PLACEMENT_3D('',#9491,#7322,#7323);
#6198=AXIS2_PLACEMENT_3D('',#9493,#7324,#7325);
#6199=AXIS2_PLACEMENT_3D('',#9494,#7326,#7327);
#6200=AXIS2_PLACEMENT_3D('',#9496,#7328,#7329);
#6201=AXIS2_PLACEMENT_3D('',#9498,#7331,#7332);
#6202=AXIS2_PLACEMENT_3D('',#9500,#7333,#7334);
#6203=AXIS2_PLACEMENT_3D('',#9501,#7335,#7336);
#6204=AXIS2_PLACEMENT_3D('',#9503,#7338,#7339);
#6205=AXIS2_PLACEMENT_3D('',#9505,#7340,#7341);
#6206=AXIS2_PLACEMENT_3D('',#9507,#7342,#7343);
#6207=AXIS2_PLACEMENT_3D('',#9508,#7344,#7345);
#6208=AXIS2_PLACEMENT_3D('',#9510,#7346,#7347);
#6209=AXIS2_PLACEMENT_3D('',#9512,#7349,#7350);
#6210=AXIS2_PLACEMENT_3D('',#9514,#7351,#7352);
#6211=AXIS2_PLACEMENT_3D('',#9515,#7353,#7354);
#6212=AXIS2_PLACEMENT_3D('',#9517,#7356,#7357);
#6213=AXIS2_PLACEMENT_3D('',#9518,#7358,#7359);
#6214=AXIS2_PLACEMENT_3D('',#9519,#7360,#7361);
#6215=AXIS2_PLACEMENT_3D('',#9520,#7362,#7363);
#6216=AXIS2_PLACEMENT_3D('',#9521,#7364,#7365);
#6217=AXIS2_PLACEMENT_3D('',#9522,#7366,#7367);
#6218=AXIS2_PLACEMENT_3D('',#9523,#7368,#7369);
#6219=AXIS2_PLACEMENT_3D('',#9525,#7370,#7371);
#6220=AXIS2_PLACEMENT_3D('',#9526,#7372,#7373);
#6221=AXIS2_PLACEMENT_3D('',#9528,#7374,#7375);
#6222=AXIS2_PLACEMENT_3D('',#9531,#7377,#7378);
#6223=AXIS2_PLACEMENT_3D('',#9532,#7379,#7380);
#6224=AXIS2_PLACEMENT_3D('',#9534,#7382,#7383);
#6225=AXIS2_PLACEMENT_3D('',#9535,#7384,#7385);
#6226=AXIS2_PLACEMENT_3D('',#9536,#7386,#7387);
#6227=AXIS2_PLACEMENT_3D('',#9545,#7392,#7393);
#6228=AXIS2_PLACEMENT_3D('',#9554,#7398,#7399);
#6229=AXIS2_PLACEMENT_3D('',#9558,#7401,#7402);
#6230=AXIS2_PLACEMENT_3D('',#9559,#7403,#7404);
#6231=AXIS2_PLACEMENT_3D('',#9569,#7405,#7406);
#6232=AXIS2_PLACEMENT_3D('',#9591,#7408,#7409);
#6233=AXIS2_PLACEMENT_3D('',#9592,#7410,#7411);
#6234=AXIS2_PLACEMENT_3D('',#9594,#7413,#7414);
#6235=AXIS2_PLACEMENT_3D('',#9596,#7415,#7416);
#6236=AXIS2_PLACEMENT_3D('',#9599,#7418,#7419);
#6237=AXIS2_PLACEMENT_3D('',#9600,#7420,#7421);
#6238=AXIS2_PLACEMENT_3D('',#9602,#7422,#7423);
#6239=AXIS2_PLACEMENT_3D('',#9603,#7424,#7425);
#6240=AXIS2_PLACEMENT_3D('',#9605,#7426,#7427);
#6241=AXIS2_PLACEMENT_3D('',#9608,#7429,#7430);
#6242=AXIS2_PLACEMENT_3D('',#9609,#7431,#7432);
#6243=AXIS2_PLACEMENT_3D('',#9611,#7433,#7434);
#6244=AXIS2_PLACEMENT_3D('',#9612,#7435,#7436);
#6245=AXIS2_PLACEMENT_3D('',#9615,#7439,#7440);
#6246=AXIS2_PLACEMENT_3D('',#9617,#7441,#7442);
#6247=AXIS2_PLACEMENT_3D('',#9619,#7444,#7445);
#6248=AXIS2_PLACEMENT_3D('',#9621,#7446,#7447);
#6249=AXIS2_PLACEMENT_3D('',#9623,#7449,#7450);
#6250=AXIS2_PLACEMENT_3D('',#9625,#7451,#7452);
#6251=AXIS2_PLACEMENT_3D('',#9629,#7455,#7456);
#6252=AXIS2_PLACEMENT_3D('',#9630,#7457,#7458);
#6253=AXIS2_PLACEMENT_3D('',#9632,#7460,#7461);
#6254=AXIS2_PLACEMENT_3D('',#9634,#7463,#7464);
#6255=AXIS2_PLACEMENT_3D('',#9635,#7465,#7466);
#6256=AXIS2_PLACEMENT_3D('',#9636,#7467,#7468);
#6257=AXIS2_PLACEMENT_3D('',#9645,#7473,#7474);
#6258=AXIS2_PLACEMENT_3D('',#9651,#7478,#7479);
#6259=AXIS2_PLACEMENT_3D('',#9657,#7483,#7484);
#6260=AXIS2_PLACEMENT_3D('',#9663,#7488,#7489);
#6261=AXIS2_PLACEMENT_3D('',#9669,#7493,#7494);
#6262=AXIS2_PLACEMENT_3D('',#9672,#7497,#7498);
#6263=AXIS2_PLACEMENT_3D('',#9673,#7499,#7500);
#6264=AXIS2_PLACEMENT_3D('',#9675,#7501,#7502);
#6265=AXIS2_PLACEMENT_3D('',#9676,#7503,#7504);
#6266=AXIS2_PLACEMENT_3D('',#9678,#7505,#7506);
#6267=AXIS2_PLACEMENT_3D('',#9680,#7508,#7509);
#6268=AXIS2_PLACEMENT_3D('',#9682,#7510,#7511);
#6269=AXIS2_PLACEMENT_3D('',#9684,#7513,#7514);
#6270=AXIS2_PLACEMENT_3D('',#9686,#7515,#7516);
#6271=AXIS2_PLACEMENT_3D('',#9688,#7518,#7519);
#6272=AXIS2_PLACEMENT_3D('',#9689,#7520,#7521);
#6273=AXIS2_PLACEMENT_3D('',#9690,#7522,#7523);
#6274=AXIS2_PLACEMENT_3D('',#9691,#7524,#7525);
#6275=AXIS2_PLACEMENT_3D('',#9693,#7526,#7527);
#6276=AXIS2_PLACEMENT_3D('',#9696,#7529,#7530);
#6277=AXIS2_PLACEMENT_3D('',#9697,#7531,#7532);
#6278=AXIS2_PLACEMENT_3D('',#9699,#7533,#7534);
#6279=AXIS2_PLACEMENT_3D('',#9702,#7536,#7537);
#6280=AXIS2_PLACEMENT_3D('',#9703,#7538,#7539);
#6281=AXIS2_PLACEMENT_3D('',#9705,#7540,#7541);
#6282=AXIS2_PLACEMENT_3D('',#9708,#7543,#7544);
#6283=AXIS2_PLACEMENT_3D('',#9709,#7545,#7546);
#6284=AXIS2_PLACEMENT_3D('',#9714,#7548,#7549);
#6285=AXIS2_PLACEMENT_3D('',#9717,#7551,#7552);
#6286=AXIS2_PLACEMENT_3D('',#9718,#7553,#7554);
#6287=AXIS2_PLACEMENT_3D('',#9724,#7558,#7559);
#6288=AXIS2_PLACEMENT_3D('',#9728,#7561,#7562);
#6289=AXIS2_PLACEMENT_3D('',#9732,#7564,#7565);
#6290=AXIS2_PLACEMENT_3D('',#9736,#7567,#7568);
#6291=AXIS2_PLACEMENT_3D('',#9740,#7570,#7571);
#6292=AXIS2_PLACEMENT_3D('',#9743,#7573,#7574);
#6293=AXIS2_PLACEMENT_3D('',#9744,#7575,#7576);
#6294=AXIS2_PLACEMENT_3D('',#9748,#7579,#7580);
#6295=AXIS2_PLACEMENT_3D('',#9751,#7582,#7583);
#6296=AXIS2_PLACEMENT_3D('',#9752,#7584,#7585);
#6297=AXIS2_PLACEMENT_3D('',#9754,#7586,#7587);
#6298=AXIS2_PLACEMENT_3D('',#9756,#7589,#7590);
#6299=AXIS2_PLACEMENT_3D('',#9761,#7593,#7594);
#6300=AXIS2_PLACEMENT_3D('',#9762,#7595,#7596);
#6301=AXIS2_PLACEMENT_3D('',#9766,#7599,#7600);
#6302=AXIS2_PLACEMENT_3D('',#9770,#7602,#7603);
#6303=AXIS2_PLACEMENT_3D('',#9773,#7605,#7606);
#6304=AXIS2_PLACEMENT_3D('',#9776,#7608,#7609);
#6305=AXIS2_PLACEMENT_3D('',#9777,#7610,#7611);
#6306=AXIS2_PLACEMENT_3D('',#9778,#7612,#7613);
#6307=AXIS2_PLACEMENT_3D('',#9781,#7616,#7617);
#6308=AXIS2_PLACEMENT_3D('',#9783,#7619,#7620);
#6309=AXIS2_PLACEMENT_3D('',#9784,#7621,#7622);
#6310=AXIS2_PLACEMENT_3D('',#9785,#7623,#7624);
#6311=AXIS2_PLACEMENT_3D('',#9787,#7625,#7626);
#6312=AXIS2_PLACEMENT_3D('',#9789,#7627,#7628);
#6313=AXIS2_PLACEMENT_3D('',#9790,#7629,#7630);
#6314=AXIS2_PLACEMENT_3D('',#9792,#7632,#7633);
#6315=AXIS2_PLACEMENT_3D('',#9795,#7635,#7636);
#6316=AXIS2_PLACEMENT_3D('',#9796,#7637,#7638);
#6317=AXIS2_PLACEMENT_3D('',#9797,#7639,#7640);
#6318=AXIS2_PLACEMENT_3D('',#9798,#7641,#7642);
#6319=AXIS2_PLACEMENT_3D('',#9800,#7643,#7644);
#6320=AXIS2_PLACEMENT_3D('',#9803,#7646,#7647);
#6321=AXIS2_PLACEMENT_3D('',#9804,#7648,#7649);
#6322=AXIS2_PLACEMENT_3D('',#9805,#7650,#7651);
#6323=AXIS2_PLACEMENT_3D('',#9807,#7652,#7653);
#6324=AXIS2_PLACEMENT_3D('',#9810,#7655,#7656);
#6325=AXIS2_PLACEMENT_3D('',#9811,#7657,#7658);
#6326=AXIS2_PLACEMENT_3D('',#9812,#7659,#7660);
#6327=AXIS2_PLACEMENT_3D('',#9813,#7661,#7662);
#6328=AXIS2_PLACEMENT_3D('',#9814,#7663,#7664);
#6329=AXIS2_PLACEMENT_3D('',#9816,#7665,#7666);
#6330=AXIS2_PLACEMENT_3D('',#9819,#7668,#7669);
#6331=AXIS2_PLACEMENT_3D('',#9820,#7670,#7671);
#6332=AXIS2_PLACEMENT_3D('',#9822,#7672,#7673);
#6333=AXIS2_PLACEMENT_3D('',#9825,#7675,#7676);
#6334=AXIS2_PLACEMENT_3D('',#9826,#7677,#7678);
#6335=AXIS2_PLACEMENT_3D('',#9827,#7679,#7680);
#6336=AXIS2_PLACEMENT_3D('',#9828,#7681,#7682);
#6337=AXIS2_PLACEMENT_3D('',#9829,#7683,#7684);
#6338=AXIS2_PLACEMENT_3D('',#9833,#7686,#7687);
#6339=AXIS2_PLACEMENT_3D('',#9834,#7688,#7689);
#6340=AXIS2_PLACEMENT_3D('',#9851,#7690,#7691);
#6341=AXIS2_PLACEMENT_3D('',#9908,#7693,#7694);
#6342=AXIS2_PLACEMENT_3D('',#9910,#7696,#7697);
#6343=AXIS2_PLACEMENT_3D('',#9912,#7698,#7699);
#6344=AXIS2_PLACEMENT_3D('',#9915,#7701,#7702);
#6345=AXIS2_PLACEMENT_3D('',#9916,#7703,#7704);
#6346=AXIS2_PLACEMENT_3D('',#9918,#7705,#7706);
#6347=AXIS2_PLACEMENT_3D('',#9921,#7708,#7709);
#6348=AXIS2_PLACEMENT_3D('',#9922,#7710,#7711);
#6349=AXIS2_PLACEMENT_3D('',#9923,#7712,#7713);
#6350=AXIS2_PLACEMENT_3D('',#9924,#7714,#7715);
#6351=AXIS2_PLACEMENT_3D('',#9925,#7716,#7717);
#6352=AXIS2_PLACEMENT_3D('',#9927,#7718,#7719);
#6353=AXIS2_PLACEMENT_3D('',#9928,#7720,#7721);
#6354=AXIS2_PLACEMENT_3D('',#9930,#7722,#7723);
#6355=AXIS2_PLACEMENT_3D('',#9932,#7725,#7726);
#6356=AXIS2_PLACEMENT_3D('',#9934,#7727,#7728);
#6357=AXIS2_PLACEMENT_3D('',#9936,#7730,#7731);
#6358=AXIS2_PLACEMENT_3D('',#9938,#7732,#7733);
#6359=AXIS2_PLACEMENT_3D('',#9940,#7735,#7736);
#6360=AXIS2_PLACEMENT_3D('',#9942,#7737,#7738);
#6361=AXIS2_PLACEMENT_3D('',#9943,#7739,#7740);
#6362=AXIS2_PLACEMENT_3D('',#9945,#7741,#7742);
#6363=AXIS2_PLACEMENT_3D('',#9947,#7744,#7745);
#6364=AXIS2_PLACEMENT_3D('',#9949,#7746,#7747);
#6365=AXIS2_PLACEMENT_3D('',#9951,#7749,#7750);
#6366=AXIS2_PLACEMENT_3D('',#9953,#7751,#7752);
#6367=AXIS2_PLACEMENT_3D('',#9955,#7754,#7755);
#6368=AXIS2_PLACEMENT_3D('',#9956,#7756,#7757);
#6369=AXIS2_PLACEMENT_3D('',#9965,#7762,#7763);
#6370=AXIS2_PLACEMENT_3D('',#9971,#7767,#7768);
#6371=AXIS2_PLACEMENT_3D('',#9977,#7772,#7773);
#6372=AXIS2_PLACEMENT_3D('',#9983,#7777,#7778);
#6373=AXIS2_PLACEMENT_3D('',#9989,#7782,#7783);
#6374=AXIS2_PLACEMENT_3D('',#9992,#7786,#7787);
#6375=AXIS2_PLACEMENT_3D('',#9993,#7788,#7789);
#6376=AXIS2_PLACEMENT_3D('',#9994,#7790,#7791);
#6377=AXIS2_PLACEMENT_3D('',#9995,#7792,#7793);
#6378=AXIS2_PLACEMENT_3D('',#9997,#7794,#7795);
#6379=AXIS2_PLACEMENT_3D('',#9998,#7796,#7797);
#6380=AXIS2_PLACEMENT_3D('',#10007,#7802,#7803);
#6381=AXIS2_PLACEMENT_3D('',#10013,#7807,#7808);
#6382=AXIS2_PLACEMENT_3D('',#10019,#7812,#7813);
#6383=AXIS2_PLACEMENT_3D('',#10025,#7817,#7818);
#6384=AXIS2_PLACEMENT_3D('',#10031,#7822,#7823);
#6385=AXIS2_PLACEMENT_3D('',#10034,#7826,#7827);
#6386=AXIS2_PLACEMENT_3D('',#10035,#7828,#7829);
#6387=AXIS2_PLACEMENT_3D('',#10037,#7830,#7831);
#6388=AXIS2_PLACEMENT_3D('',#10038,#7832,#7833);
#6389=AXIS2_PLACEMENT_3D('',#10040,#7834,#7835);
#6390=AXIS2_PLACEMENT_3D('',#10042,#7837,#7838);
#6391=AXIS2_PLACEMENT_3D('',#10044,#7840,#7841);
#6392=AXIS2_PLACEMENT_3D('',#10045,#7842,#7843);
#6393=AXIS2_PLACEMENT_3D('',#10047,#7844,#7845);
#6394=AXIS2_PLACEMENT_3D('',#10050,#7847,#7848);
#6395=AXIS2_PLACEMENT_3D('',#10051,#7849,#7850);
#6396=AXIS2_PLACEMENT_3D('',#10052,#7851,#7852);
#6397=AXIS2_PLACEMENT_3D('',#10054,#7853,#7854);
#6398=AXIS2_PLACEMENT_3D('',#10056,#7855,#7856);
#6399=AXIS2_PLACEMENT_3D('',#10057,#7857,#7858);
#6400=AXIS2_PLACEMENT_3D('',#10059,#7859,#7860);
#6401=AXIS2_PLACEMENT_3D('',#10061,#7861,#7862);
#6402=AXIS2_PLACEMENT_3D('',#10062,#7863,#7864);
#6403=AXIS2_PLACEMENT_3D('',#10064,#7866,#7867);
#6404=AXIS2_PLACEMENT_3D('',#10067,#7869,#7870);
#6405=AXIS2_PLACEMENT_3D('',#10068,#7871,#7872);
#6406=AXIS2_PLACEMENT_3D('',#10070,#7873,#7874);
#6407=AXIS2_PLACEMENT_3D('',#10072,#7876,#7877);
#6408=AXIS2_PLACEMENT_3D('',#10073,#7878,#7879);
#6409=AXIS2_PLACEMENT_3D('',#10074,#7880,#7881);
#6410=AXIS2_PLACEMENT_3D('',#10075,#7882,#7883);
#6411=AXIS2_PLACEMENT_3D('',#10077,#7884,#7885);
#6412=AXIS2_PLACEMENT_3D('',#10080,#7887,#7888);
#6413=AXIS2_PLACEMENT_3D('',#10081,#7889,#7890);
#6414=AXIS2_PLACEMENT_3D('',#10083,#7891,#7892);
#6415=AXIS2_PLACEMENT_3D('',#10086,#7894,#7895);
#6416=AXIS2_PLACEMENT_3D('',#10087,#7896,#7897);
#6417=AXIS2_PLACEMENT_3D('',#10088,#7898,#7899);
#6418=AXIS2_PLACEMENT_3D('',#10089,#7900,#7901);
#6419=AXIS2_PLACEMENT_3D('',#10090,#7902,#7903);
#6420=AXIS2_PLACEMENT_3D('',#10091,#7904,#7905);
#6421=AXIS2_PLACEMENT_3D('',#10093,#7906,#7907);
#6422=AXIS2_PLACEMENT_3D('',#10096,#7909,#7910);
#6423=AXIS2_PLACEMENT_3D('',#10097,#7911,#7912);
#6424=AXIS2_PLACEMENT_3D('',#10099,#7913,#7914);
#6425=AXIS2_PLACEMENT_3D('',#10102,#7916,#7917);
#6426=AXIS2_PLACEMENT_3D('',#10103,#7918,#7919);
#6427=AXIS2_PLACEMENT_3D('',#10108,#7921,#7922);
#6428=AXIS2_PLACEMENT_3D('',#10111,#7924,#7925);
#6429=AXIS2_PLACEMENT_3D('',#10112,#7926,#7927);
#6430=AXIS2_PLACEMENT_3D('',#10118,#7931,#7932);
#6431=AXIS2_PLACEMENT_3D('',#10121,#7934,#7935);
#6432=AXIS2_PLACEMENT_3D('',#10122,#7936,#7937);
#6433=AXIS2_PLACEMENT_3D('',#10126,#7940,#7941);
#6434=AXIS2_PLACEMENT_3D('',#10127,#7942,#7943);
#6435=AXIS2_PLACEMENT_3D('',#10128,#7944,#7945);
#6436=AXIS2_PLACEMENT_3D('',#10129,#7946,#7947);
#6437=AXIS2_PLACEMENT_3D('',#10130,#7948,#7949);
#6438=AXIS2_PLACEMENT_3D('',#10132,#7950,#7951);
#6439=AXIS2_PLACEMENT_3D('',#10135,#7953,#7954);
#6440=AXIS2_PLACEMENT_3D('',#10136,#7955,#7956);
#6441=AXIS2_PLACEMENT_3D('',#10138,#7957,#7958);
#6442=AXIS2_PLACEMENT_3D('',#10141,#7960,#7961);
#6443=AXIS2_PLACEMENT_3D('',#10142,#7962,#7963);
#6444=AXIS2_PLACEMENT_3D('',#10143,#7964,#7965);
#6445=AXIS2_PLACEMENT_3D('',#10144,#7966,#7967);
#6446=AXIS2_PLACEMENT_3D('',#10145,#7968,#7969);
#6447=AXIS2_PLACEMENT_3D('',#10146,#7970,#7971);
#6448=AXIS2_PLACEMENT_3D('',#10147,#7972,#7973);
#6449=AXIS2_PLACEMENT_3D('',#10148,#7974,#7975);
#6450=AXIS2_PLACEMENT_3D('',#10149,#7976,#7977);
#6451=AXIS2_PLACEMENT_3D('',#10151,#7978,#7979);
#6452=AXIS2_PLACEMENT_3D('',#10154,#7981,#7982);
#6453=AXIS2_PLACEMENT_3D('',#10155,#7983,#7984);
#6454=AXIS2_PLACEMENT_3D('',#10156,#7985,#7986);
#6455=AXIS2_PLACEMENT_3D('',#10158,#7987,#7988);
#6456=AXIS2_PLACEMENT_3D('',#10160,#7989,#7990);
#6457=AXIS2_PLACEMENT_3D('',#10161,#7991,#7992);
#6458=AXIS2_PLACEMENT_3D('',#10163,#7993,#7994);
#6459=AXIS2_PLACEMENT_3D('',#10165,#7995,#7996);
#6460=AXIS2_PLACEMENT_3D('',#10166,#7997,#7998);
#6461=AXIS2_PLACEMENT_3D('',#10168,#8000,#8001);
#6462=AXIS2_PLACEMENT_3D('',#10171,#8003,#8004);
#6463=AXIS2_PLACEMENT_3D('',#10172,#8005,#8006);
#6464=AXIS2_PLACEMENT_3D('',#10174,#8007,#8008);
#6465=AXIS2_PLACEMENT_3D('',#10176,#8010,#8011);
#6466=AXIS2_PLACEMENT_3D('',#10177,#8012,#8013);
#6467=AXIS2_PLACEMENT_3D('',#10178,#8014,#8015);
#6468=AXIS2_PLACEMENT_3D('',#10179,#8016,#8017);
#6469=AXIS2_PLACEMENT_3D('',#10181,#8018,#8019);
#6470=AXIS2_PLACEMENT_3D('',#10184,#8021,#8022);
#6471=AXIS2_PLACEMENT_3D('',#10185,#8023,#8024);
#6472=AXIS2_PLACEMENT_3D('',#10187,#8025,#8026);
#6473=AXIS2_PLACEMENT_3D('',#10190,#8028,#8029);
#6474=AXIS2_PLACEMENT_3D('',#10191,#8030,#8031);
#6475=AXIS2_PLACEMENT_3D('',#10192,#8032,#8033);
#6476=AXIS2_PLACEMENT_3D('',#10193,#8034,#8035);
#6477=AXIS2_PLACEMENT_3D('',#10194,#8036,#8037);
#6478=AXIS2_PLACEMENT_3D('',#10196,#8038,#8039);
#6479=AXIS2_PLACEMENT_3D('',#10199,#8041,#8042);
#6480=AXIS2_PLACEMENT_3D('',#10200,#8043,#8044);
#6481=AXIS2_PLACEMENT_3D('',#10201,#8045,#8046);
#6482=AXIS2_PLACEMENT_3D('',#10203,#8047,#8048);
#6483=AXIS2_PLACEMENT_3D('',#10206,#8050,#8051);
#6484=AXIS2_PLACEMENT_3D('',#10207,#8052,#8053);
#6485=AXIS2_PLACEMENT_3D('',#10209,#8054,#8055);
#6486=AXIS2_PLACEMENT_3D('',#10212,#8057,#8058);
#6487=AXIS2_PLACEMENT_3D('',#10213,#8059,#8060);
#6488=AXIS2_PLACEMENT_3D('',#10215,#8061,#8062);
#6489=AXIS2_PLACEMENT_3D('',#10218,#8064,#8065);
#6490=AXIS2_PLACEMENT_3D('',#10219,#8066,#8067);
#6491=AXIS2_PLACEMENT_3D('',#10221,#8068,#8069);
#6492=AXIS2_PLACEMENT_3D('',#10224,#8071,#8072);
#6493=AXIS2_PLACEMENT_3D('',#10225,#8073,#8074);
#6494=AXIS2_PLACEMENT_3D('',#10227,#8075,#8076);
#6495=AXIS2_PLACEMENT_3D('',#10230,#8078,#8079);
#6496=AXIS2_PLACEMENT_3D('',#10231,#8080,#8081);
#6497=AXIS2_PLACEMENT_3D('',#10240,#8086,#8087);
#6498=AXIS2_PLACEMENT_3D('',#10246,#8091,#8092);
#6499=AXIS2_PLACEMENT_3D('',#10252,#8096,#8097);
#6500=AXIS2_PLACEMENT_3D('',#10255,#8100,#8101);
#6501=AXIS2_PLACEMENT_3D('',#10256,#8102,#8103);
#6502=AXIS2_PLACEMENT_3D('',#10257,#8104,#8105);
#6503=AXIS2_PLACEMENT_3D('',#10258,#8106,#8107);
#6504=AXIS2_PLACEMENT_3D('',#10259,#8108,#8109);
#6505=AXIS2_PLACEMENT_3D('',#10262,#8110,#8111);
#6506=AXIS2_PLACEMENT_3D('',#10268,#8115,#8116);
#6507=AXIS2_PLACEMENT_3D('',#10274,#8120,#8121);
#6508=AXIS2_PLACEMENT_3D('',#10276,#8122,#8123);
#6509=AXIS2_PLACEMENT_3D('',#10280,#8126,#8127);
#6510=AXIS2_PLACEMENT_3D('',#10283,#8130,#8131);
#6511=AXIS2_PLACEMENT_3D('',#10284,#8132,#8133);
#6512=AXIS2_PLACEMENT_3D('',#10286,#8134,#8135);
#6513=AXIS2_PLACEMENT_3D('',#10288,#8136,#8137);
#6514=AXIS2_PLACEMENT_3D('',#10289,#8138,#8139);
#6515=AXIS2_PLACEMENT_3D('',#10291,#8140,#8141);
#6516=AXIS2_PLACEMENT_3D('',#10293,#8143,#8144);
#6517=AXIS2_PLACEMENT_3D('',#10295,#8145,#8146);
#6518=AXIS2_PLACEMENT_3D('',#10296,#8147,#8148);
#6519=AXIS2_PLACEMENT_3D('',#10298,#8149,#8150);
#6520=AXIS2_PLACEMENT_3D('',#10300,#8152,#8153);
#6521=AXIS2_PLACEMENT_3D('',#10302,#8154,#8155);
#6522=AXIS2_PLACEMENT_3D('',#10303,#8156,#8157);
#6523=AXIS2_PLACEMENT_3D('',#10305,#8158,#8159);
#6524=AXIS2_PLACEMENT_3D('',#10307,#8161,#8162);
#6525=AXIS2_PLACEMENT_3D('',#10309,#8163,#8164);
#6526=AXIS2_PLACEMENT_3D('',#10310,#8165,#8166);
#6527=AXIS2_PLACEMENT_3D('',#10312,#8167,#8168);
#6528=AXIS2_PLACEMENT_3D('',#10314,#8170,#8171);
#6529=AXIS2_PLACEMENT_3D('',#10316,#8172,#8173);
#6530=AXIS2_PLACEMENT_3D('',#10317,#8174,#8175);
#6531=AXIS2_PLACEMENT_3D('',#10319,#8176,#8177);
#6532=AXIS2_PLACEMENT_3D('',#10321,#8179,#8180);
#6533=AXIS2_PLACEMENT_3D('',#10323,#8181,#8182);
#6534=AXIS2_PLACEMENT_3D('',#10324,#8183,#8184);
#6535=AXIS2_PLACEMENT_3D('',#10326,#8186,#8187);
#6536=AXIS2_PLACEMENT_3D('',#10327,#8188,#8189);
#6537=AXIS2_PLACEMENT_3D('',#10330,#8190,#8191);
#6538=AXIS2_PLACEMENT_3D('',#10334,#8193,#8194);
#6539=AXIS2_PLACEMENT_3D('',#10336,#8196,#8197);
#6540=AXIS2_PLACEMENT_3D('',#10342,#8201,#8202);
#6541=AXIS2_PLACEMENT_3D('',#10344,#8203,#8204);
#6542=AXIS2_PLACEMENT_3D('',#10346,#8205,#8206);
#6543=AXIS2_PLACEMENT_3D('',#10348,#8208,#8209);
#6544=AXIS2_PLACEMENT_3D('',#10351,#8212,#8213);
#6545=AXIS2_PLACEMENT_3D('',#10353,#8214,#8215);
#6546=AXIS2_PLACEMENT_3D('',#10355,#8216,#8217);
#6547=AXIS2_PLACEMENT_3D('',#10356,#8218,#8219);
#6548=AXIS2_PLACEMENT_3D('',#10358,#8220,#8221);
#6549=AXIS2_PLACEMENT_3D('',#10360,#8223,#8224);
#6550=AXIS2_PLACEMENT_3D('',#10362,#8225,#8226);
#6551=AXIS2_PLACEMENT_3D('',#10363,#8227,#8228);
#6552=AXIS2_PLACEMENT_3D('',#10365,#8230,#8231);
#6553=AXIS2_PLACEMENT_3D('',#10366,#8232,#8233);
#6554=AXIS2_PLACEMENT_3D('',#10367,#8234,#8235);
#6555=AXIS2_PLACEMENT_3D('',#10368,#8236,#8237);
#6556=AXIS2_PLACEMENT_3D('',#10370,#8238,#8239);
#6557=AXIS2_PLACEMENT_3D('',#10373,#8241,#8242);
#6558=AXIS2_PLACEMENT_3D('',#10374,#8243,#8244);
#6559=AXIS2_PLACEMENT_3D('',#10376,#8245,#8246);
#6560=AXIS2_PLACEMENT_3D('',#10379,#8248,#8249);
#6561=AXIS2_PLACEMENT_3D('',#10380,#8250,#8251);
#6562=AXIS2_PLACEMENT_3D('',#10382,#8252,#8253);
#6563=AXIS2_PLACEMENT_3D('',#10385,#8255,#8256);
#6564=AXIS2_PLACEMENT_3D('',#10386,#8257,#8258);
#6565=AXIS2_PLACEMENT_3D('',#10388,#8259,#8260);
#6566=AXIS2_PLACEMENT_3D('',#10391,#8262,#8263);
#6567=AXIS2_PLACEMENT_3D('',#10392,#8264,#8265);
#6568=AXIS2_PLACEMENT_3D('',#10394,#8266,#8267);
#6569=AXIS2_PLACEMENT_3D('',#10397,#8269,#8270);
#6570=AXIS2_PLACEMENT_3D('',#10398,#8271,#8272);
#6571=AXIS2_PLACEMENT_3D('',#10407,#8277,#8278);
#6572=AXIS2_PLACEMENT_3D('',#10413,#8282,#8283);
#6573=AXIS2_PLACEMENT_3D('',#10419,#8287,#8288);
#6574=AXIS2_PLACEMENT_3D('',#10422,#8291,#8292);
#6575=AXIS2_PLACEMENT_3D('',#10423,#8293,#8294);
#6576=AXIS2_PLACEMENT_3D('',#10424,#8295,#8296);
#6577=AXIS2_PLACEMENT_3D('',#10425,#8297,#8298);
#6578=AXIS2_PLACEMENT_3D('',#10427,#8299,#8300);
#6579=AXIS2_PLACEMENT_3D('',#10430,#8302,#8303);
#6580=AXIS2_PLACEMENT_3D('',#10431,#8304,#8305);
#6581=AXIS2_PLACEMENT_3D('',#10433,#8306,#8307);
#6582=AXIS2_PLACEMENT_3D('',#10436,#8309,#8310);
#6583=AXIS2_PLACEMENT_3D('',#10437,#8311,#8312);
#6584=AXIS2_PLACEMENT_3D('',#10438,#8313,#8314);
#6585=AXIS2_PLACEMENT_3D('',#10439,#8315,#8316);
#6586=AXIS2_PLACEMENT_3D('',#10440,#8317,#8318);
#6587=AXIS2_PLACEMENT_3D('',#10442,#8319,#8320);
#6588=AXIS2_PLACEMENT_3D('',#10445,#8322,#8323);
#6589=AXIS2_PLACEMENT_3D('',#10446,#8324,#8325);
#6590=AXIS2_PLACEMENT_3D('',#10448,#8326,#8327);
#6591=AXIS2_PLACEMENT_3D('',#10451,#8329,#8330);
#6592=AXIS2_PLACEMENT_3D('',#10452,#8331,#8332);
#6593=AXIS2_PLACEMENT_3D('',#10453,#8333,#8334);
#6594=AXIS2_PLACEMENT_3D('',#10454,#8335,#8336);
#6595=AXIS2_PLACEMENT_3D('',#10455,#8337,#8338);
#6596=AXIS2_PLACEMENT_3D('',#10464,#8343,#8344);
#6597=AXIS2_PLACEMENT_3D('',#10470,#8348,#8349);
#6598=AXIS2_PLACEMENT_3D('',#10476,#8353,#8354);
#6599=AXIS2_PLACEMENT_3D('',#10482,#8358,#8359);
#6600=AXIS2_PLACEMENT_3D('',#10488,#8363,#8364);
#6601=AXIS2_PLACEMENT_3D('',#10491,#8367,#8368);
#6602=AXIS2_PLACEMENT_3D('',#10492,#8369,#8370);
#6603=AXIS2_PLACEMENT_3D('',#10493,#8371,#8372);
#6604=AXIS2_PLACEMENT_3D('',#10495,#8373,#8374);
#6605=AXIS2_PLACEMENT_3D('',#10496,#8375,#8376);
#6606=AXIS2_PLACEMENT_3D('',#10498,#8377,#8378);
#6607=AXIS2_PLACEMENT_3D('',#10499,#8379,#8380);
#6608=AXIS2_PLACEMENT_3D('',#10501,#8381,#8382);
#6609=AXIS2_PLACEMENT_3D('',#10503,#8384,#8385);
#6610=AXIS2_PLACEMENT_3D('',#10505,#8386,#8387);
#6611=AXIS2_PLACEMENT_3D('',#10507,#8389,#8390);
#6612=AXIS2_PLACEMENT_3D('',#10509,#8391,#8392);
#6613=AXIS2_PLACEMENT_3D('',#10511,#8394,#8395);
#6614=AXIS2_PLACEMENT_3D('',#10513,#8396,#8397);
#6615=AXIS2_PLACEMENT_3D('',#10514,#8398,#8399);
#6616=AXIS2_PLACEMENT_3D('',#10516,#8400,#8401);
#6617=AXIS2_PLACEMENT_3D('',#10518,#8403,#8404);
#6618=AXIS2_PLACEMENT_3D('',#10520,#8406,#8407);
#6619=AXIS2_PLACEMENT_3D('',#10521,#8408,#8409);
#6620=AXIS2_PLACEMENT_3D('',#10522,#8410,#8411);
#6621=AXIS2_PLACEMENT_3D('',#10523,#8412,#8413);
#6622=AXIS2_PLACEMENT_3D('',#10524,#8414,#8415);
#6623=AXIS2_PLACEMENT_3D('',#10525,#8416,#8417);
#6624=AXIS2_PLACEMENT_3D('',#10526,#8418,#8419);
#6625=AXIS2_PLACEMENT_3D('',#10527,#8420,#8421);
#6626=AXIS2_PLACEMENT_3D('',#10528,#8422,#8423);
#6627=AXIS2_PLACEMENT_3D('',#10529,#8424,#8425);
#6628=AXIS2_PLACEMENT_3D('',#10530,#8426,#8427);
#6629=AXIS2_PLACEMENT_3D('',#10531,#8428,#8429);
#6630=AXIS2_PLACEMENT_3D('',#10532,#8430,#8431);
#6631=AXIS2_PLACEMENT_3D('',#10533,#8432,#8433);
#6632=AXIS2_PLACEMENT_3D('',#10534,#8434,#8435);
#6633=AXIS2_PLACEMENT_3D('',#10535,#8436,#8437);
#6634=AXIS2_PLACEMENT_3D('',#10536,#8438,#8439);
#6635=AXIS2_PLACEMENT_3D('',#10537,#8440,#8441);
#6636=AXIS2_PLACEMENT_3D('',#10538,#8442,#8443);
#6637=AXIS2_PLACEMENT_3D('',#10539,#8444,#8445);
#6638=AXIS2_PLACEMENT_3D('',#10540,#8446,#8447);
#6639=AXIS2_PLACEMENT_3D('',#10541,#8448,#8449);
#6640=AXIS2_PLACEMENT_3D('',#10542,#8450,#8451);
#6641=AXIS2_PLACEMENT_3D('',#10543,#8452,#8453);
#6642=AXIS2_PLACEMENT_3D('',#10544,#8454,#8455);
#6643=AXIS2_PLACEMENT_3D('',#10545,#8456,#8457);
#6644=AXIS2_PLACEMENT_3D('',#10546,#8458,#8459);
#6645=AXIS2_PLACEMENT_3D('',#10547,#8460,#8461);
#6646=AXIS2_PLACEMENT_3D('',#10548,#8462,#8463);
#6647=AXIS2_PLACEMENT_3D('',#10549,#8464,#8465);
#6648=AXIS2_PLACEMENT_3D('',#10550,#8466,#8467);
#6649=AXIS2_PLACEMENT_3D('',#10551,#8468,#8469);
#6650=AXIS2_PLACEMENT_3D('',#10552,#8470,#8471);
#6651=AXIS2_PLACEMENT_3D('',#10553,#8472,#8473);
#6652=AXIS2_PLACEMENT_3D('',#10554,#8474,#8475);
#6653=AXIS2_PLACEMENT_3D('',#10555,#8476,#8477);
#6654=AXIS2_PLACEMENT_3D('',#10556,#8478,#8479);
#6655=AXIS2_PLACEMENT_3D('',#10557,#8480,#8481);
#6656=AXIS2_PLACEMENT_3D('',#10558,#8482,#8483);
#6657=AXIS2_PLACEMENT_3D('',#10559,#8484,#8485);
#6658=AXIS2_PLACEMENT_3D('',#10560,#8486,#8487);
#6659=AXIS2_PLACEMENT_3D('',#10561,#8488,#8489);
#6660=AXIS2_PLACEMENT_3D('',#10562,#8490,#8491);
#6661=AXIS2_PLACEMENT_3D('',#10563,#8492,#8493);
#6662=AXIS2_PLACEMENT_3D('',#10564,#8494,#8495);
#6663=AXIS2_PLACEMENT_3D('',#10565,#8496,#8497);
#6664=AXIS2_PLACEMENT_3D('',#10566,#8498,#8499);
#6665=AXIS2_PLACEMENT_3D('',#10567,#8500,#8501);
#6666=AXIS2_PLACEMENT_3D('',#10568,#8502,#8503);
#6667=AXIS2_PLACEMENT_3D('',#10569,#8504,#8505);
#6668=AXIS2_PLACEMENT_3D('',#10570,#8506,#8507);
#6669=AXIS2_PLACEMENT_3D('',#10571,#8508,#8509);
#6670=AXIS2_PLACEMENT_3D('',#10572,#8510,#8511);
#6671=DIRECTION('axis',(0.,0.,1.));
#6672=DIRECTION('refdir',(1.,0.,0.));
#6673=DIRECTION('axis',(0.,0.,1.));
#6674=DIRECTION('refdir',(1.,0.,0.));
#6675=DIRECTION('axis',(0.,0.,1.));
#6676=DIRECTION('refdir',(1.,0.,0.));
#6677=DIRECTION('center_axis',(0.,0.,1.));
#6678=DIRECTION('ref_axis',(1.,0.,0.));
#6679=DIRECTION('center_axis',(0.,0.,1.));
#6680=DIRECTION('ref_axis',(1.,0.,0.));
#6681=DIRECTION('',(0.,0.,1.));
#6682=DIRECTION('center_axis',(0.,0.,-1.));
#6683=DIRECTION('ref_axis',(1.,0.,0.));
#6684=DIRECTION('center_axis',(0.,0.,1.));
#6685=DIRECTION('ref_axis',(1.,0.,0.));
#6686=DIRECTION('center_axis',(0.,0.,1.));
#6687=DIRECTION('ref_axis',(1.,0.,0.));
#6688=DIRECTION('',(0.,0.,1.));
#6689=DIRECTION('center_axis',(0.,0.,-1.));
#6690=DIRECTION('ref_axis',(1.,0.,0.));
#6691=DIRECTION('center_axis',(0.,0.,1.));
#6692=DIRECTION('ref_axis',(1.,0.,0.));
#6693=DIRECTION('center_axis',(0.,0.,1.));
#6694=DIRECTION('ref_axis',(1.,0.,0.));
#6695=DIRECTION('',(0.,0.,1.));
#6696=DIRECTION('center_axis',(0.,0.,-1.));
#6697=DIRECTION('ref_axis',(1.,0.,0.));
#6698=DIRECTION('center_axis',(0.,0.,1.));
#6699=DIRECTION('ref_axis',(1.,0.,0.));
#6700=DIRECTION('center_axis',(0.,0.,1.));
#6701=DIRECTION('ref_axis',(1.,0.,0.));
#6702=DIRECTION('',(0.,0.,1.));
#6703=DIRECTION('center_axis',(0.,0.,-1.));
#6704=DIRECTION('ref_axis',(1.,0.,0.));
#6705=DIRECTION('center_axis',(0.,0.,1.));
#6706=DIRECTION('ref_axis',(1.,0.,0.));
#6707=DIRECTION('center_axis',(0.,0.,1.));
#6708=DIRECTION('ref_axis',(1.,0.,0.));
#6709=DIRECTION('',(0.,0.,1.));
#6710=DIRECTION('center_axis',(0.,0.,-1.));
#6711=DIRECTION('ref_axis',(1.,0.,0.));
#6712=DIRECTION('center_axis',(0.,0.,1.));
#6713=DIRECTION('ref_axis',(1.,0.,0.));
#6714=DIRECTION('center_axis',(0.,0.,1.));
#6715=DIRECTION('ref_axis',(1.,0.,0.));
#6716=DIRECTION('',(0.,0.,1.));
#6717=DIRECTION('center_axis',(0.,0.,-1.));
#6718=DIRECTION('ref_axis',(1.,0.,0.));
#6719=DIRECTION('center_axis',(0.,0.,1.));
#6720=DIRECTION('ref_axis',(1.,0.,0.));
#6721=DIRECTION('center_axis',(0.,0.,1.));
#6722=DIRECTION('ref_axis',(1.,0.,0.));
#6723=DIRECTION('',(0.,0.,1.));
#6724=DIRECTION('center_axis',(0.,0.,-1.));
#6725=DIRECTION('ref_axis',(1.,0.,0.));
#6726=DIRECTION('center_axis',(0.,0.,1.));
#6727=DIRECTION('ref_axis',(1.,0.,0.));
#6728=DIRECTION('center_axis',(0.,0.,1.));
#6729=DIRECTION('ref_axis',(1.,0.,0.));
#6730=DIRECTION('',(0.,0.,1.));
#6731=DIRECTION('center_axis',(0.,0.,-1.));
#6732=DIRECTION('ref_axis',(1.,0.,0.));
#6733=DIRECTION('center_axis',(0.,1.,0.));
#6734=DIRECTION('ref_axis',(-1.,0.,0.));
#6735=DIRECTION('',(-1.,0.,0.));
#6736=DIRECTION('',(0.,0.,1.));
#6737=DIRECTION('',(-1.,0.,0.));
#6738=DIRECTION('',(0.,0.,1.));
#6739=DIRECTION('center_axis',(1.,0.,0.));
#6740=DIRECTION('ref_axis',(0.,1.,0.));
#6741=DIRECTION('',(0.,1.,0.));
#6742=DIRECTION('',(0.,1.,0.));
#6743=DIRECTION('',(0.,0.,1.));
#6744=DIRECTION('center_axis',(0.,-1.,0.));
#6745=DIRECTION('ref_axis',(1.,0.,0.));
#6746=DIRECTION('',(1.,0.,0.));
#6747=DIRECTION('',(1.,0.,0.));
#6748=DIRECTION('',(0.,0.,1.));
#6749=DIRECTION('center_axis',(-1.,0.,0.));
#6750=DIRECTION('ref_axis',(0.,-1.,0.));
#6751=DIRECTION('',(0.,-1.,0.));
#6752=DIRECTION('',(0.,-1.,0.));
#6753=DIRECTION('center_axis',(0.,0.,1.));
#6754=DIRECTION('ref_axis',(1.,0.,0.));
#6755=DIRECTION('center_axis',(0.,0.,1.));
#6756=DIRECTION('ref_axis',(1.,0.,0.));
#6757=DIRECTION('axis',(0.,0.,1.));
#6758=DIRECTION('refdir',(1.,0.,0.));
#6759=DIRECTION('center_axis',(0.866025403784439,0.,-0.5));
#6760=DIRECTION('ref_axis',(0.5,0.,0.866025403784439));
#6761=DIRECTION('',(-0.5,0.,-0.866025403784439));
#6762=DIRECTION('',(0.,-1.,0.));
#6763=DIRECTION('',(0.5,0.,0.866025403784439));
#6764=DIRECTION('',(0.,-1.,0.));
#6765=DIRECTION('center_axis',(1.20185167898973E-16,0.,-1.));
#6766=DIRECTION('ref_axis',(1.,0.,1.20185167898973E-16));
#6767=DIRECTION('',(-1.,0.,-1.20185167898973E-16));
#6768=DIRECTION('',(0.,-1.,0.));
#6769=DIRECTION('',(1.,0.,1.20185167898973E-16));
#6770=DIRECTION('center_axis',(-0.866025403784439,0.,-0.5));
#6771=DIRECTION('ref_axis',(0.5,0.,-0.866025403784439));
#6772=DIRECTION('',(-0.5,0.,0.866025403784439));
#6773=DIRECTION('',(0.,-1.,0.));
#6774=DIRECTION('',(0.5,0.,-0.866025403784439));
#6775=DIRECTION('center_axis',(-0.866025403784439,0.,0.5));
#6776=DIRECTION('ref_axis',(-0.5,0.,-0.866025403784439));
#6777=DIRECTION('',(0.5,0.,0.866025403784439));
#6778=DIRECTION('',(0.,-1.,0.));
#6779=DIRECTION('',(-0.5,0.,-0.866025403784439));
#6780=DIRECTION('center_axis',(-2.40370335797945E-16,0.,1.));
#6781=DIRECTION('ref_axis',(-1.,0.,-2.40370335797945E-16));
#6782=DIRECTION('',(1.,0.,2.40370335797945E-16));
#6783=DIRECTION('',(0.,-1.,0.));
#6784=DIRECTION('',(-1.,0.,-2.40370335797945E-16));
#6785=DIRECTION('center_axis',(0.866025403784439,0.,0.5));
#6786=DIRECTION('ref_axis',(-0.5,0.,0.866025403784439));
#6787=DIRECTION('',(0.5,0.,-0.866025403784439));
#6788=DIRECTION('',(-0.5,0.,0.866025403784439));
#6789=DIRECTION('center_axis',(0.,1.,0.));
#6790=DIRECTION('ref_axis',(1.,0.,0.));
#6791=DIRECTION('center_axis',(0.,-1.,0.));
#6792=DIRECTION('ref_axis',(0.,0.,-1.));
#6793=DIRECTION('center_axis',(0.,1.,0.));
#6794=DIRECTION('ref_axis',(1.,0.,0.));
#6795=DIRECTION('center_axis',(0.,1.,0.));
#6796=DIRECTION('ref_axis',(1.,0.,0.));
#6797=DIRECTION('center_axis',(0.,1.,0.));
#6798=DIRECTION('ref_axis',(0.,0.,1.));
#6799=DIRECTION('center_axis',(0.,-1.,0.));
#6800=DIRECTION('ref_axis',(1.,0.,0.));
#6801=DIRECTION('center_axis',(0.,-1.,0.));
#6802=DIRECTION('ref_axis',(1.,0.,0.));
#6803=DIRECTION('center_axis',(0.,-1.,0.));
#6804=DIRECTION('ref_axis',(1.,0.,0.));
#6805=DIRECTION('',(0.707106781186548,0.707106781186547,8.65956056235493E-17));
#6806=DIRECTION('center_axis',(0.,-1.,0.));
#6807=DIRECTION('ref_axis',(1.,0.,0.));
#6808=DIRECTION('center_axis',(0.,-1.,0.));
#6809=DIRECTION('ref_axis',(1.,0.,0.));
#6810=DIRECTION('',(0.,1.,0.));
#6811=DIRECTION('center_axis',(0.,1.,0.));
#6812=DIRECTION('ref_axis',(1.,0.,0.));
#6813=DIRECTION('center_axis',(0.,-1.,0.));
#6814=DIRECTION('ref_axis',(1.,0.,0.));
#6815=DIRECTION('',(-0.707106781186547,0.707106781186548,-8.65956056235493E-17));
#6816=DIRECTION('center_axis',(0.,-1.,0.));
#6817=DIRECTION('ref_axis',(0.,0.,-1.));
#6818=DIRECTION('center_axis',(0.,-1.,0.));
#6819=DIRECTION('ref_axis',(1.,0.,0.));
#6820=DIRECTION('center_axis',(0.,1.,0.));
#6821=DIRECTION('ref_axis',(1.,0.,0.));
#6822=DIRECTION('center_axis',(0.,1.,0.));
#6823=DIRECTION('ref_axis',(1.,0.,0.));
#6824=DIRECTION('',(-0.447213595499958,0.894427190999916,-5.47678698264203E-17));
#6825=DIRECTION('center_axis',(0.,-1.,0.));
#6826=DIRECTION('ref_axis',(1.,0.,0.));
#6827=DIRECTION('',(0.,1.,0.));
#6828=DIRECTION('axis',(0.,0.,1.));
#6829=DIRECTION('refdir',(1.,0.,0.));
#6830=DIRECTION('center_axis',(1.,0.,0.));
#6831=DIRECTION('ref_axis',(0.,0.,-1.));
#6832=DIRECTION('',(1.,0.,0.));
#6833=DIRECTION('center_axis',(0.,0.,1.));
#6834=DIRECTION('ref_axis',(1.,0.,0.));
#6835=DIRECTION('center_axis',(0.,0.,1.));
#6836=DIRECTION('ref_axis',(1.,0.,0.));
#6837=DIRECTION('',(0.,0.,1.));
#6838=DIRECTION('center_axis',(0.,0.,-1.));
#6839=DIRECTION('ref_axis',(1.,0.,0.));
#6840=DIRECTION('center_axis',(0.,0.,1.));
#6841=DIRECTION('ref_axis',(1.,0.,0.));
#6842=DIRECTION('center_axis',(0.,0.,1.));
#6843=DIRECTION('ref_axis',(1.,0.,0.));
#6844=DIRECTION('center_axis',(0.,0.,1.));
#6845=DIRECTION('ref_axis',(1.,0.,0.));
#6846=DIRECTION('',(0.,0.,1.));
#6847=DIRECTION('center_axis',(0.,0.,-1.));
#6848=DIRECTION('ref_axis',(1.,0.,0.));
#6849=DIRECTION('center_axis',(0.,0.,1.));
#6850=DIRECTION('ref_axis',(1.,0.,0.));
#6851=DIRECTION('center_axis',(0.,0.,1.));
#6852=DIRECTION('ref_axis',(1.,0.,0.));
#6853=DIRECTION('center_axis',(0.,0.,1.));
#6854=DIRECTION('ref_axis',(1.,0.,0.));
#6855=DIRECTION('',(0.,0.,1.));
#6856=DIRECTION('center_axis',(0.,0.,-1.));
#6857=DIRECTION('ref_axis',(1.,0.,0.));
#6858=DIRECTION('center_axis',(0.,0.,1.));
#6859=DIRECTION('ref_axis',(1.,0.,0.));
#6860=DIRECTION('center_axis',(0.,0.,1.));
#6861=DIRECTION('ref_axis',(1.,0.,0.));
#6862=DIRECTION('center_axis',(0.,0.,1.));
#6863=DIRECTION('ref_axis',(1.,0.,0.));
#6864=DIRECTION('',(0.,0.,1.));
#6865=DIRECTION('center_axis',(0.,0.,-1.));
#6866=DIRECTION('ref_axis',(1.,0.,0.));
#6867=DIRECTION('center_axis',(0.,0.,1.));
#6868=DIRECTION('ref_axis',(1.,0.,0.));
#6869=DIRECTION('center_axis',(0.,0.,1.));
#6870=DIRECTION('ref_axis',(1.,0.,0.));
#6871=DIRECTION('center_axis',(0.,0.,1.));
#6872=DIRECTION('ref_axis',(1.,0.,0.));
#6873=DIRECTION('center_axis',(0.,0.,1.));
#6874=DIRECTION('ref_axis',(1.,0.,0.));
#6875=DIRECTION('center_axis',(0.,0.,1.));
#6876=DIRECTION('ref_axis',(1.,0.,0.));
#6877=DIRECTION('',(0.,0.,1.));
#6878=DIRECTION('center_axis',(0.,0.,1.));
#6879=DIRECTION('ref_axis',(1.,0.,0.));
#6880=DIRECTION('',(0.,0.,-1.));
#6881=DIRECTION('center_axis',(0.,0.,1.));
#6882=DIRECTION('ref_axis',(1.,0.,0.));
#6883=DIRECTION('',(0.,0.,-1.));
#6884=DIRECTION('center_axis',(0.,0.,1.));
#6885=DIRECTION('ref_axis',(1.,0.,0.));
#6886=DIRECTION('',(0.,0.,1.));
#6887=DIRECTION('center_axis',(0.,0.,1.));
#6888=DIRECTION('ref_axis',(1.,0.,0.));
#6889=DIRECTION('center_axis',(0.,0.,1.));
#6890=DIRECTION('ref_axis',(1.,0.,0.));
#6891=DIRECTION('center_axis',(0.,0.,1.));
#6892=DIRECTION('ref_axis',(1.,0.,0.));
#6893=DIRECTION('center_axis',(0.,0.,1.));
#6894=DIRECTION('ref_axis',(-0.707106781186548,-0.707106781186547,0.));
#6895=DIRECTION('',(0.,0.,-1.));
#6896=DIRECTION('center_axis',(0.,0.,1.));
#6897=DIRECTION('ref_axis',(1.,0.,0.));
#6898=DIRECTION('',(0.,0.,1.));
#6899=DIRECTION('center_axis',(0.,0.,1.));
#6900=DIRECTION('ref_axis',(1.,0.,0.));
#6901=DIRECTION('center_axis',(0.,0.,1.));
#6902=DIRECTION('ref_axis',(1.,0.,0.));
#6903=DIRECTION('center_axis',(0.,0.,1.));
#6904=DIRECTION('ref_axis',(1.,0.,0.));
#6905=DIRECTION('center_axis',(0.,0.,1.));
#6906=DIRECTION('ref_axis',(-0.707106781186547,0.707106781186548,0.));
#6907=DIRECTION('',(0.,0.,-1.));
#6908=DIRECTION('center_axis',(0.,0.,1.));
#6909=DIRECTION('ref_axis',(1.,0.,0.));
#6910=DIRECTION('',(0.,0.,1.));
#6911=DIRECTION('center_axis',(0.,0.,1.));
#6912=DIRECTION('ref_axis',(1.,0.,0.));
#6913=DIRECTION('center_axis',(0.,0.,1.));
#6914=DIRECTION('ref_axis',(1.,0.,0.));
#6915=DIRECTION('center_axis',(0.,0.,1.));
#6916=DIRECTION('ref_axis',(1.,0.,0.));
#6917=DIRECTION('center_axis',(0.,0.,1.));
#6918=DIRECTION('ref_axis',(1.,0.,0.));
#6919=DIRECTION('center_axis',(0.,0.,1.));
#6920=DIRECTION('ref_axis',(1.,0.,0.));
#6921=DIRECTION('',(0.,0.,-1.));
#6922=DIRECTION('center_axis',(0.,0.,1.));
#6923=DIRECTION('ref_axis',(1.,0.,0.));
#6924=DIRECTION('center_axis',(0.,0.,1.));
#6925=DIRECTION('ref_axis',(1.,0.,0.));
#6926=DIRECTION('center_axis',(0.,0.,1.));
#6927=DIRECTION('ref_axis',(1.,0.,0.));
#6928=DIRECTION('center_axis',(0.,0.,1.));
#6929=DIRECTION('ref_axis',(1.,0.,0.));
#6930=DIRECTION('center_axis',(0.,0.,1.));
#6931=DIRECTION('ref_axis',(1.,0.,0.));
#6932=DIRECTION('center_axis',(0.,0.,1.));
#6933=DIRECTION('ref_axis',(1.,0.,0.));
#6934=DIRECTION('center_axis',(0.,0.,1.));
#6935=DIRECTION('ref_axis',(1.,0.,0.));
#6936=DIRECTION('center_axis',(0.,0.,-1.));
#6937=DIRECTION('ref_axis',(1.,0.,0.));
#6938=DIRECTION('center_axis',(0.,0.,-1.));
#6939=DIRECTION('ref_axis',(1.,0.,0.));
#6940=DIRECTION('center_axis',(0.,0.,-1.));
#6941=DIRECTION('ref_axis',(1.,0.,0.));
#6942=DIRECTION('center_axis',(0.,0.,-1.));
#6943=DIRECTION('ref_axis',(1.,0.,0.));
#6944=DIRECTION('center_axis',(0.,0.,1.));
#6945=DIRECTION('ref_axis',(1.,0.,0.));
#6946=DIRECTION('center_axis',(0.,0.,1.));
#6947=DIRECTION('ref_axis',(1.,0.,0.));
#6948=DIRECTION('',(0.,0.,1.));
#6949=DIRECTION('center_axis',(0.,0.,1.));
#6950=DIRECTION('ref_axis',(1.,0.,0.));
#6951=DIRECTION('center_axis',(0.,0.,1.));
#6952=DIRECTION('ref_axis',(1.,0.,0.));
#6953=DIRECTION('',(0.,0.,1.));
#6954=DIRECTION('center_axis',(0.,0.,1.));
#6955=DIRECTION('ref_axis',(1.,0.,0.));
#6956=DIRECTION('center_axis',(0.,0.,1.));
#6957=DIRECTION('ref_axis',(1.,0.,0.));
#6958=DIRECTION('',(0.,0.,1.));
#6959=DIRECTION('center_axis',(0.,0.,1.));
#6960=DIRECTION('ref_axis',(1.,0.,0.));
#6961=DIRECTION('center_axis',(0.,0.,1.));
#6962=DIRECTION('ref_axis',(1.,0.,0.));
#6963=DIRECTION('',(0.,0.,1.));
#6964=DIRECTION('center_axis',(0.,0.,1.));
#6965=DIRECTION('ref_axis',(1.,0.,0.));
#6966=DIRECTION('center_axis',(0.,0.,1.));
#6967=DIRECTION('ref_axis',(1.,0.,0.));
#6968=DIRECTION('',(0.,0.,1.));
#6969=DIRECTION('center_axis',(0.,0.,-1.));
#6970=DIRECTION('ref_axis',(1.,0.,0.));
#6971=DIRECTION('center_axis',(0.,0.,1.));
#6972=DIRECTION('ref_axis',(1.,0.,0.));
#6973=DIRECTION('center_axis',(0.,0.,1.));
#6974=DIRECTION('ref_axis',(1.,0.,0.));
#6975=DIRECTION('center_axis',(0.,0.,1.));
#6976=DIRECTION('ref_axis',(1.,0.,0.));
#6977=DIRECTION('',(0.,0.,-1.));
#6978=DIRECTION('center_axis',(0.,0.,1.));
#6979=DIRECTION('ref_axis',(1.,0.,0.));
#6980=DIRECTION('center_axis',(0.,0.,1.));
#6981=DIRECTION('ref_axis',(1.,0.,0.));
#6982=DIRECTION('',(0.,0.,-1.));
#6983=DIRECTION('center_axis',(0.,0.,-1.));
#6984=DIRECTION('ref_axis',(1.,0.,0.));
#6985=DIRECTION('center_axis',(0.,0.,1.));
#6986=DIRECTION('ref_axis',(1.,0.,0.));
#6987=DIRECTION('center_axis',(0.,0.,1.));
#6988=DIRECTION('ref_axis',(1.,0.,0.));
#6989=DIRECTION('axis',(0.,0.,1.));
#6990=DIRECTION('refdir',(1.,0.,0.));
#6991=DIRECTION('center_axis',(0.,0.,1.));
#6992=DIRECTION('ref_axis',(1.,0.,0.));
#6993=DIRECTION('center_axis',(0.,0.,1.));
#6994=DIRECTION('ref_axis',(1.,0.,0.));
#6995=DIRECTION('',(0.,0.,1.));
#6996=DIRECTION('center_axis',(0.,0.,-1.));
#6997=DIRECTION('ref_axis',(1.,0.,0.));
#6998=DIRECTION('center_axis',(0.,0.,1.));
#6999=DIRECTION('ref_axis',(1.,0.,0.));
#7000=DIRECTION('center_axis',(0.,0.,1.));
#7001=DIRECTION('ref_axis',(1.,0.,0.));
#7002=DIRECTION('center_axis',(0.,0.,1.));
#7003=DIRECTION('ref_axis',(1.,0.,0.));
#7004=DIRECTION('center_axis',(0.,0.,1.));
#7005=DIRECTION('ref_axis',(1.,0.,0.));
#7006=DIRECTION('',(0.,0.,1.));
#7007=DIRECTION('center_axis',(0.,0.,-1.));
#7008=DIRECTION('ref_axis',(1.,0.,0.));
#7009=DIRECTION('center_axis',(0.,0.,1.));
#7010=DIRECTION('ref_axis',(1.,0.,0.));
#7011=DIRECTION('center_axis',(0.,0.,1.));
#7012=DIRECTION('ref_axis',(1.,0.,0.));
#7013=DIRECTION('center_axis',(0.,0.,1.));
#7014=DIRECTION('ref_axis',(1.,0.,0.));
#7015=DIRECTION('center_axis',(0.,0.,1.));
#7016=DIRECTION('ref_axis',(1.,0.,0.));
#7017=DIRECTION('',(0.,0.,1.));
#7018=DIRECTION('center_axis',(0.,0.,-1.));
#7019=DIRECTION('ref_axis',(1.,0.,0.));
#7020=DIRECTION('center_axis',(0.,0.,1.));
#7021=DIRECTION('ref_axis',(1.,0.,0.));
#7022=DIRECTION('center_axis',(0.,0.,1.));
#7023=DIRECTION('ref_axis',(1.,0.,0.));
#7024=DIRECTION('center_axis',(0.,0.,1.));
#7025=DIRECTION('ref_axis',(1.,0.,0.));
#7026=DIRECTION('center_axis',(0.,0.,1.));
#7027=DIRECTION('ref_axis',(1.,0.,0.));
#7028=DIRECTION('',(0.,0.,1.));
#7029=DIRECTION('center_axis',(0.,0.,-1.));
#7030=DIRECTION('ref_axis',(1.,0.,0.));
#7031=DIRECTION('center_axis',(0.,0.,1.));
#7032=DIRECTION('ref_axis',(1.,0.,0.));
#7033=DIRECTION('center_axis',(0.,0.,1.));
#7034=DIRECTION('ref_axis',(1.,0.,0.));
#7035=DIRECTION('center_axis',(0.,0.,1.));
#7036=DIRECTION('ref_axis',(1.,0.,0.));
#7037=DIRECTION('center_axis',(0.,0.,1.));
#7038=DIRECTION('ref_axis',(1.,0.,0.));
#7039=DIRECTION('',(0.,0.,1.));
#7040=DIRECTION('center_axis',(0.,0.,1.));
#7041=DIRECTION('ref_axis',(1.,0.,0.));
#7042=DIRECTION('center_axis',(0.,0.,1.));
#7043=DIRECTION('ref_axis',(1.,0.,0.));
#7044=DIRECTION('',(0.,0.,1.));
#7045=DIRECTION('center_axis',(0.,0.,1.));
#7046=DIRECTION('ref_axis',(1.,0.,0.));
#7047=DIRECTION('center_axis',(0.,0.,1.));
#7048=DIRECTION('ref_axis',(1.,0.,0.));
#7049=DIRECTION('',(0.,0.,1.));
#7050=DIRECTION('center_axis',(0.,0.,1.));
#7051=DIRECTION('ref_axis',(1.,0.,0.));
#7052=DIRECTION('center_axis',(0.,0.,1.));
#7053=DIRECTION('ref_axis',(1.,0.,0.));
#7054=DIRECTION('',(0.,0.,1.));
#7055=DIRECTION('center_axis',(0.,0.,1.));
#7056=DIRECTION('ref_axis',(1.,0.,0.));
#7057=DIRECTION('center_axis',(0.,0.,1.));
#7058=DIRECTION('ref_axis',(1.,0.,0.));
#7059=DIRECTION('',(0.,0.,-1.));
#7060=DIRECTION('center_axis',(0.,0.,1.));
#7061=DIRECTION('ref_axis',(1.,0.,0.));
#7062=DIRECTION('center_axis',(0.,0.,1.));
#7063=DIRECTION('ref_axis',(1.,0.,0.));
#7064=DIRECTION('center_axis',(0.,0.,-1.));
#7065=DIRECTION('ref_axis',(1.,0.,0.));
#7066=DIRECTION('center_axis',(0.,0.,1.));
#7067=DIRECTION('ref_axis',(1.,0.,0.));
#7068=DIRECTION('center_axis',(0.,0.,-1.));
#7069=DIRECTION('ref_axis',(1.,0.,0.));
#7070=DIRECTION('',(0.,0.,-1.));
#7071=DIRECTION('center_axis',(0.,0.,1.));
#7072=DIRECTION('ref_axis',(1.,0.,0.));
#7073=DIRECTION('center_axis',(0.,0.,1.));
#7074=DIRECTION('ref_axis',(1.,0.,0.));
#7075=DIRECTION('',(0.,0.,-1.));
#7076=DIRECTION('center_axis',(0.,0.,1.));
#7077=DIRECTION('ref_axis',(1.,0.,0.));
#7078=DIRECTION('center_axis',(0.,0.,1.));
#7079=DIRECTION('ref_axis',(1.,0.,0.));
#7080=DIRECTION('center_axis',(0.,0.,1.));
#7081=DIRECTION('ref_axis',(1.,0.,0.));
#7082=DIRECTION('axis',(0.,0.,1.));
#7083=DIRECTION('refdir',(1.,0.,0.));
#7084=DIRECTION('axis',(0.,0.,1.));
#7085=DIRECTION('refdir',(1.,0.,0.));
#7086=DIRECTION('center_axis',(0.,-1.,0.));
#7087=DIRECTION('ref_axis',(0.,0.,-1.));
#7088=DIRECTION('center_axis',(0.,-1.,0.));
#7089=DIRECTION('ref_axis',(1.,0.,0.));
#7090=DIRECTION('center_axis',(0.,-1.,0.));
#7091=DIRECTION('ref_axis',(1.,0.,0.));
#7092=DIRECTION('center_axis',(1.,0.,1.22464679914735E-16));
#7093=DIRECTION('ref_axis',(-1.22464679914735E-16,0.,1.));
#7094=DIRECTION('center_axis',(0.,1.,0.));
#7095=DIRECTION('ref_axis',(1.,0.,0.));
#7096=DIRECTION('center_axis',(0.,1.,0.));
#7097=DIRECTION('ref_axis',(1.,0.,0.));
#7098=DIRECTION('center_axis',(0.,-1.,0.));
#7099=DIRECTION('ref_axis',(1.,0.,0.));
#7100=DIRECTION('',(0.,1.,0.));
#7101=DIRECTION('center_axis',(0.,-1.,0.));
#7102=DIRECTION('ref_axis',(1.,0.,0.));
#7103=DIRECTION('center_axis',(0.,-1.,0.));
#7104=DIRECTION('ref_axis',(1.,0.,0.));
#7105=DIRECTION('center_axis',(0.,-1.,0.));
#7106=DIRECTION('ref_axis',(1.,0.,0.));
#7107=DIRECTION('',(0.,1.,0.));
#7108=DIRECTION('center_axis',(0.,-1.,0.));
#7109=DIRECTION('ref_axis',(1.,0.,0.));
#7110=DIRECTION('center_axis',(0.,1.,0.));
#7111=DIRECTION('ref_axis',(1.,0.,0.));
#7112=DIRECTION('',(-0.707106781186547,0.707106781186548,-8.65956056235493E-17));
#7113=DIRECTION('center_axis',(0.,-1.,0.));
#7114=DIRECTION('ref_axis',(1.,0.,0.));
#7115=DIRECTION('center_axis',(0.,1.,0.));
#7116=DIRECTION('ref_axis',(0.,0.,1.));
#7117=DIRECTION('center_axis',(0.,-1.,0.));
#7118=DIRECTION('ref_axis',(1.,0.,0.));
#7119=DIRECTION('center_axis',(0.,-1.,0.));
#7120=DIRECTION('ref_axis',(1.,0.,0.));
#7121=DIRECTION('',(0.,1.,0.));
#7122=DIRECTION('center_axis',(0.,-1.,0.));
#7123=DIRECTION('ref_axis',(0.,0.,-1.));
#7124=DIRECTION('center_axis',(0.,-1.,0.));
#7125=DIRECTION('ref_axis',(1.,0.,0.));
#7126=DIRECTION('center_axis',(0.,-1.,0.));
#7127=DIRECTION('ref_axis',(1.,0.,0.));
#7128=DIRECTION('',(0.707106781186547,0.707106781186548,8.65956056235493E-17));
#7129=DIRECTION('axis',(0.,0.,1.));
#7130=DIRECTION('refdir',(1.,0.,0.));
#7131=DIRECTION('center_axis',(0.,-1.,0.));
#7132=DIRECTION('ref_axis',(0.,0.,-1.));
#7133=DIRECTION('center_axis',(0.,-1.,0.));
#7134=DIRECTION('ref_axis',(1.,0.,0.));
#7135=DIRECTION('center_axis',(0.,-1.,0.));
#7136=DIRECTION('ref_axis',(1.,0.,0.));
#7137=DIRECTION('center_axis',(1.,0.,1.22464679914735E-16));
#7138=DIRECTION('ref_axis',(-1.22464679914735E-16,0.,1.));
#7139=DIRECTION('center_axis',(0.,1.,0.));
#7140=DIRECTION('ref_axis',(1.,0.,0.));
#7141=DIRECTION('center_axis',(0.,1.,0.));
#7142=DIRECTION('ref_axis',(1.,0.,0.));
#7143=DIRECTION('center_axis',(0.,-1.,0.));
#7144=DIRECTION('ref_axis',(1.,0.,0.));
#7145=DIRECTION('center_axis',(0.,-1.,0.));
#7146=DIRECTION('ref_axis',(1.,0.,0.));
#7147=DIRECTION('',(0.,1.,0.));
#7148=DIRECTION('center_axis',(0.,1.,0.));
#7149=DIRECTION('ref_axis',(0.,0.,1.));
#7150=DIRECTION('center_axis',(0.,-1.,0.));
#7151=DIRECTION('ref_axis',(1.,0.,0.));
#7152=DIRECTION('center_axis',(0.,-1.,0.));
#7153=DIRECTION('ref_axis',(1.,0.,0.));
#7154=DIRECTION('center_axis',(0.,-1.,0.));
#7155=DIRECTION('ref_axis',(1.,0.,0.));
#7156=DIRECTION('center_axis',(0.,-1.,0.));
#7157=DIRECTION('ref_axis',(1.,0.,0.));
#7158=DIRECTION('',(0.707106781186548,0.707106781186547,8.65956056235494E-17));
#7159=DIRECTION('center_axis',(0.,-1.,0.));
#7160=DIRECTION('ref_axis',(1.,0.,0.));
#7161=DIRECTION('center_axis',(0.,-1.,0.));
#7162=DIRECTION('ref_axis',(1.,0.,0.));
#7163=DIRECTION('',(0.,1.,0.));
#7164=DIRECTION('center_axis',(0.,1.,0.));
#7165=DIRECTION('ref_axis',(1.,0.,0.));
#7166=DIRECTION('center_axis',(0.,-1.,0.));
#7167=DIRECTION('ref_axis',(1.,0.,0.));
#7168=DIRECTION('',(-0.707106781186548,0.707106781186547,-8.65956056235494E-17));
#7169=DIRECTION('center_axis',(0.,-1.,0.));
#7170=DIRECTION('ref_axis',(0.,0.,-1.));
#7171=DIRECTION('center_axis',(0.,-1.,0.));
#7172=DIRECTION('ref_axis',(1.,0.,0.));
#7173=DIRECTION('',(0.,1.,0.));
#7174=DIRECTION('axis',(0.,0.,1.));
#7175=DIRECTION('refdir',(1.,0.,0.));
#7176=DIRECTION('center_axis',(0.,0.,1.));
#7177=DIRECTION('ref_axis',(1.,0.,0.));
#7178=DIRECTION('center_axis',(1.22464679914735E-16,-1.,0.));
#7179=DIRECTION('ref_axis',(-1.,-1.22464679914735E-16,0.));
#7180=DIRECTION('center_axis',(0.707106781186548,0.,0.707106781186548));
#7181=DIRECTION('ref_axis',(0.707106781186548,0.,-0.707106781186548));
#7182=DIRECTION('center_axis',(8.65956056235494E-17,-1.,-8.65956056235493E-17));
#7183=DIRECTION('ref_axis',(-0.707106781186547,-1.22464679914735E-16,0.707106781186547));
#7184=DIRECTION('center_axis',(1.,0.,0.));
#7185=DIRECTION('ref_axis',(6.12323399573676E-17,0.,-1.));
#7186=DIRECTION('center_axis',(7.49879891330929E-33,-1.,-1.22464679914735E-16));
#7187=DIRECTION('ref_axis',(-6.12323399573676E-17,-1.22464679914735E-16,
1.));
#7188=DIRECTION('center_axis',(0.707106781186548,0.,-0.707106781186548));
#7189=DIRECTION('ref_axis',(-0.707106781186548,0.,-0.707106781186548));
#7190=DIRECTION('center_axis',(-8.65956056235493E-17,-1.,-8.65956056235494E-17));
#7191=DIRECTION('ref_axis',(0.707106781186547,-1.22464679914735E-16,0.707106781186547));
#7192=DIRECTION('center_axis',(0.,0.,-1.));
#7193=DIRECTION('ref_axis',(-1.,0.,-1.22464679914735E-16));
#7194=DIRECTION('center_axis',(-1.22464679914735E-16,-1.,-1.49975978266186E-32));
#7195=DIRECTION('ref_axis',(1.,-1.22464679914735E-16,1.22464679914735E-16));
#7196=DIRECTION('center_axis',(-0.707106781186547,0.,-0.707106781186548));
#7197=DIRECTION('ref_axis',(-0.707106781186548,0.,0.707106781186547));
#7198=DIRECTION('center_axis',(-8.65956056235493E-17,-1.,8.65956056235493E-17));
#7199=DIRECTION('ref_axis',(0.707106781186548,-1.22464679914735E-16,-0.707106781186547));
#7200=DIRECTION('center_axis',(-1.,0.,0.));
#7201=DIRECTION('ref_axis',(-1.83697019872103E-16,0.,1.));
#7202=DIRECTION('center_axis',(-2.24963967399279E-32,-1.,1.22464679914735E-16));
#7203=DIRECTION('ref_axis',(1.83697019872103E-16,-1.22464679914735E-16,
-1.));
#7204=DIRECTION('center_axis',(-0.707106781186548,0.,0.707106781186548));
#7205=DIRECTION('ref_axis',(0.707106781186547,0.,0.707106781186548));
#7206=DIRECTION('center_axis',(8.65956056235493E-17,-1.,8.65956056235493E-17));
#7207=DIRECTION('ref_axis',(-0.707106781186547,-1.22464679914735E-16,-0.707106781186548));
#7208=DIRECTION('axis',(0.,0.,1.));
#7209=DIRECTION('refdir',(1.,0.,0.));
#7210=DIRECTION('center_axis',(0.,0.,1.));
#7211=DIRECTION('ref_axis',(1.,0.,0.));
#7212=DIRECTION('center_axis',(0.,-1.,0.));
#7213=DIRECTION('ref_axis',(0.,0.,-1.));
#7214=DIRECTION('center_axis',(0.,-1.,0.));
#7215=DIRECTION('ref_axis',(0.,0.,-1.));
#7216=DIRECTION('center_axis',(0.,1.,0.));
#7217=DIRECTION('ref_axis',(1.,0.,0.));
#7218=DIRECTION('center_axis',(0.,1.,0.));
#7219=DIRECTION('ref_axis',(1.,0.,0.));
#7220=DIRECTION('center_axis',(0.,1.,0.));
#7221=DIRECTION('ref_axis',(1.,0.,0.));
#7222=DIRECTION('center_axis',(0.,1.,0.));
#7223=DIRECTION('ref_axis',(1.,0.,0.));
#7224=DIRECTION('',(0.,-1.,0.));
#7225=DIRECTION('center_axis',(0.,-1.,0.));
#7226=DIRECTION('ref_axis',(1.,0.,0.));
#7227=DIRECTION('center_axis',(0.,1.,0.));
#7228=DIRECTION('ref_axis',(1.,0.,0.));
#7229=DIRECTION('center_axis',(0.,1.,0.));
#7230=DIRECTION('ref_axis',(1.,0.,0.));
#7231=DIRECTION('center_axis',(0.,1.,0.));
#7232=DIRECTION('ref_axis',(1.,0.,0.));
#7233=DIRECTION('center_axis',(0.,1.,0.));
#7234=DIRECTION('ref_axis',(1.,0.,0.));
#7235=DIRECTION('center_axis',(0.,1.,0.));
#7236=DIRECTION('ref_axis',(1.,0.,0.));
#7237=DIRECTION('center_axis',(0.,1.,0.));
#7238=DIRECTION('ref_axis',(1.,0.,0.));
#7239=DIRECTION('center_axis',(0.,-1.,0.));
#7240=DIRECTION('ref_axis',(1.,0.,0.));
#7241=DIRECTION('center_axis',(0.,-1.,0.));
#7242=DIRECTION('ref_axis',(0.,0.,-1.));
#7243=DIRECTION('center_axis',(6.12323399573677E-17,0.,1.));
#7244=DIRECTION('ref_axis',(1.,0.,0.));
#7245=DIRECTION('center_axis',(0.,-1.,0.));
#7246=DIRECTION('ref_axis',(0.,0.,-1.));
#7247=DIRECTION('center_axis',(0.,1.,0.));
#7248=DIRECTION('ref_axis',(1.,0.,0.));
#7249=DIRECTION('center_axis',(0.,-1.,0.));
#7250=DIRECTION('ref_axis',(1.,0.,0.));
#7251=DIRECTION('center_axis',(0.,-1.,0.));
#7252=DIRECTION('ref_axis',(0.,0.,-1.));
#7253=DIRECTION('center_axis',(0.,0.,1.));
#7254=DIRECTION('ref_axis',(1.,0.,0.));
#7255=DIRECTION('center_axis',(0.,-1.,0.));
#7256=DIRECTION('ref_axis',(0.,0.,-1.));
#7257=DIRECTION('center_axis',(0.,1.,0.));
#7258=DIRECTION('ref_axis',(1.,0.,0.));
#7259=DIRECTION('center_axis',(0.,-1.,0.));
#7260=DIRECTION('ref_axis',(1.,0.,0.));
#7261=DIRECTION('center_axis',(0.,-1.,0.));
#7262=DIRECTION('ref_axis',(0.,0.,-1.));
#7263=DIRECTION('center_axis',(0.,0.,1.));
#7264=DIRECTION('ref_axis',(1.,0.,0.));
#7265=DIRECTION('center_axis',(0.,-1.,0.));
#7266=DIRECTION('ref_axis',(0.,0.,-1.));
#7267=DIRECTION('center_axis',(0.,1.,0.));
#7268=DIRECTION('ref_axis',(1.,0.,0.));
#7269=DIRECTION('center_axis',(0.,-1.,0.));
#7270=DIRECTION('ref_axis',(1.,0.,0.));
#7271=DIRECTION('center_axis',(0.,-1.,0.));
#7272=DIRECTION('ref_axis',(0.,0.,-1.));
#7273=DIRECTION('center_axis',(0.,0.,1.));
#7274=DIRECTION('ref_axis',(1.,0.,0.));
#7275=DIRECTION('center_axis',(0.,-1.,0.));
#7276=DIRECTION('ref_axis',(0.,0.,-1.));
#7277=DIRECTION('center_axis',(0.,1.,0.));
#7278=DIRECTION('ref_axis',(1.,0.,0.));
#7279=DIRECTION('center_axis',(0.,-1.,0.));
#7280=DIRECTION('ref_axis',(1.,0.,0.));
#7281=DIRECTION('center_axis',(0.,-1.,0.));
#7282=DIRECTION('ref_axis',(0.,0.,-1.));
#7283=DIRECTION('center_axis',(6.12323399573676E-17,0.,1.));
#7284=DIRECTION('ref_axis',(1.,0.,0.));
#7285=DIRECTION('center_axis',(0.,-1.,0.));
#7286=DIRECTION('ref_axis',(0.,0.,-1.));
#7287=DIRECTION('center_axis',(0.,1.,0.));
#7288=DIRECTION('ref_axis',(1.,0.,0.));
#7289=DIRECTION('center_axis',(0.,-1.,0.));
#7290=DIRECTION('ref_axis',(1.,0.,0.));
#7291=DIRECTION('center_axis',(0.,-1.,0.));
#7292=DIRECTION('ref_axis',(0.,0.,-1.));
#7293=DIRECTION('center_axis',(0.,0.,1.));
#7294=DIRECTION('ref_axis',(1.,0.,0.));
#7295=DIRECTION('center_axis',(0.,-1.,0.));
#7296=DIRECTION('ref_axis',(0.,0.,-1.));
#7297=DIRECTION('center_axis',(0.,1.,0.));
#7298=DIRECTION('ref_axis',(1.,0.,0.));
#7299=DIRECTION('center_axis',(0.,1.,0.));
#7300=DIRECTION('ref_axis',(1.,0.,0.));
#7301=DIRECTION('',(0.,1.,0.));
#7302=DIRECTION('center_axis',(0.,-1.,0.));
#7303=DIRECTION('ref_axis',(1.,0.,0.));
#7304=DIRECTION('center_axis',(0.,-1.,0.));
#7305=DIRECTION('ref_axis',(1.,0.,0.));
#7306=DIRECTION('center_axis',(0.,1.,0.));
#7307=DIRECTION('ref_axis',(1.,0.,0.));
#7308=DIRECTION('center_axis',(0.,-1.,0.));
#7309=DIRECTION('ref_axis',(0.,0.,-1.));
#7310=DIRECTION('center_axis',(0.,0.,1.));
#7311=DIRECTION('ref_axis',(1.,0.,0.));
#7312=DIRECTION('center_axis',(0.,-1.,0.));
#7313=DIRECTION('ref_axis',(0.,0.,-1.));
#7314=DIRECTION('center_axis',(0.,-1.,0.));
#7315=DIRECTION('ref_axis',(-1.,0.,0.));
#7316=DIRECTION('center_axis',(0.,1.,0.));
#7317=DIRECTION('ref_axis',(1.,0.,0.));
#7318=DIRECTION('axis',(0.,0.,1.));
#7319=DIRECTION('refdir',(1.,0.,0.));
#7320=DIRECTION('center_axis',(0.,1.,0.));
#7321=DIRECTION('ref_axis',(0.,0.,1.));
#7322=DIRECTION('center_axis',(0.,-1.,0.));
#7323=DIRECTION('ref_axis',(1.,0.,0.));
#7324=DIRECTION('center_axis',(0.,-1.,0.));
#7325=DIRECTION('ref_axis',(1.,0.,0.));
#7326=DIRECTION('center_axis',(0.,-1.,0.));
#7327=DIRECTION('ref_axis',(1.,0.,0.));
#7328=DIRECTION('center_axis',(0.,-1.,0.));
#7329=DIRECTION('ref_axis',(1.,0.,0.));
#7330=DIRECTION('',(0.,1.,0.));
#7331=DIRECTION('center_axis',(0.,-1.,0.));
#7332=DIRECTION('ref_axis',(0.,0.,-1.));
#7333=DIRECTION('center_axis',(0.,-1.,0.));
#7334=DIRECTION('ref_axis',(1.,0.,0.));
#7335=DIRECTION('center_axis',(0.,-1.,0.));
#7336=DIRECTION('ref_axis',(1.,0.,0.));
#7337=DIRECTION('',(0.,1.,0.));
#7338=DIRECTION('center_axis',(0.,1.,0.));
#7339=DIRECTION('ref_axis',(0.,0.,1.));
#7340=DIRECTION('center_axis',(0.,-1.,0.));
#7341=DIRECTION('ref_axis',(1.,0.,0.));
#7342=DIRECTION('center_axis',(0.,-1.,0.));
#7343=DIRECTION('ref_axis',(1.,0.,0.));
#7344=DIRECTION('center_axis',(0.,-1.,0.));
#7345=DIRECTION('ref_axis',(1.,0.,0.));
#7346=DIRECTION('center_axis',(0.,-1.,0.));
#7347=DIRECTION('ref_axis',(1.,0.,0.));
#7348=DIRECTION('',(0.,1.,0.));
#7349=DIRECTION('center_axis',(0.,-1.,0.));
#7350=DIRECTION('ref_axis',(0.,0.,-1.));
#7351=DIRECTION('center_axis',(0.,-1.,0.));
#7352=DIRECTION('ref_axis',(1.,0.,0.));
#7353=DIRECTION('center_axis',(0.,-1.,0.));
#7354=DIRECTION('ref_axis',(1.,0.,0.));
#7355=DIRECTION('',(0.,1.,0.));
#7356=DIRECTION('',(0.,0.,1.));
#7357=DIRECTION('',(1.,0.,0.));
#7358=DIRECTION('',(0.,0.,1.));
#7359=DIRECTION('',(1.,0.,0.));
#7360=DIRECTION('',(0.,0.,1.));
#7361=DIRECTION('',(1.,0.,0.));
#7362=DIRECTION('',(0.,0.,1.));
#7363=DIRECTION('',(1.,0.,0.));
#7364=DIRECTION('',(0.,0.,1.));
#7365=DIRECTION('',(1.,0.,0.));
#7366=DIRECTION('axis',(0.,0.,1.));
#7367=DIRECTION('refdir',(1.,0.,0.));
#7368=DIRECTION('center_axis',(1.,0.,0.));
#7369=DIRECTION('ref_axis',(0.,0.,-1.));
#7370=DIRECTION('center_axis',(-1.,0.,0.));
#7371=DIRECTION('ref_axis',(0.,0.,-1.));
#7372=DIRECTION('center_axis',(1.,0.,0.));
#7373=DIRECTION('ref_axis',(0.,0.,-1.));
#7374=DIRECTION('center_axis',(-1.,0.,0.));
#7375=DIRECTION('ref_axis',(0.,0.,-1.));
#7376=DIRECTION('',(-0.707106781186548,8.65956056235493E-17,-0.707106781186547));
#7377=DIRECTION('center_axis',(1.,0.,0.));
#7378=DIRECTION('ref_axis',(0.,0.,-1.));
#7379=DIRECTION('center_axis',(1.,0.,0.));
#7380=DIRECTION('ref_axis',(0.,0.,-1.));
#7381=DIRECTION('',(-1.,0.,0.));
#7382=DIRECTION('center_axis',(1.,0.,0.));
#7383=DIRECTION('ref_axis',(0.,0.,-1.));
#7384=DIRECTION('axis',(0.,0.,1.));
#7385=DIRECTION('refdir',(1.,0.,0.));
#7386=DIRECTION('center_axis',(0.,1.,0.));
#7387=DIRECTION('ref_axis',(0.,0.,1.));
#7388=DIRECTION('',(-1.,0.,0.));
#7389=DIRECTION('',(0.,0.,1.));
#7390=DIRECTION('',(1.,0.,0.));
#7391=DIRECTION('',(0.,0.,-1.));
#7392=DIRECTION('center_axis',(0.,-1.,0.));
#7393=DIRECTION('ref_axis',(0.,0.,-1.));
#7394=DIRECTION('',(1.,0.,0.));
#7395=DIRECTION('',(0.,0.,1.));
#7396=DIRECTION('',(-1.,0.,0.));
#7397=DIRECTION('',(0.,0.,-1.));
#7398=DIRECTION('center_axis',(0.,0.,1.));
#7399=DIRECTION('ref_axis',(1.,0.,0.));
#7400=DIRECTION('',(1.,0.,0.));
#7401=DIRECTION('center_axis',(0.,0.,1.));
#7402=DIRECTION('ref_axis',(1.,0.,0.));
#7403=DIRECTION('center_axis',(0.,0.,1.));
#7404=DIRECTION('ref_axis',(1.,0.,0.));
#7405=DIRECTION('center_axis',(0.,0.,1.));
#7406=DIRECTION('ref_axis',(1.,0.,0.));
#7407=DIRECTION('',(0.,0.,1.));
#7408=DIRECTION('center_axis',(0.,0.,-1.));
#7409=DIRECTION('ref_axis',(1.,0.,0.));
#7410=DIRECTION('center_axis',(0.,0.,1.));
#7411=DIRECTION('ref_axis',(1.,0.,0.));
#7412=DIRECTION('',(-1.,0.,0.));
#7413=DIRECTION('center_axis',(0.,0.,1.));
#7414=DIRECTION('ref_axis',(1.,0.,0.));
#7415=DIRECTION('center_axis',(0.,0.,1.));
#7416=DIRECTION('ref_axis',(1.,0.,0.));
#7417=DIRECTION('',(0.,0.,1.));
#7418=DIRECTION('center_axis',(0.,0.,-1.));
#7419=DIRECTION('ref_axis',(1.,0.,0.));
#7420=DIRECTION('center_axis',(0.,0.,1.));
#7421=DIRECTION('ref_axis',(1.,0.,0.));
#7422=DIRECTION('center_axis',(0.,0.,1.));
#7423=DIRECTION('ref_axis',(1.,0.,0.));
#7424=DIRECTION('center_axis',(0.,0.,1.));
#7425=DIRECTION('ref_axis',(1.,0.,0.));
#7426=DIRECTION('center_axis',(0.,0.,1.));
#7427=DIRECTION('ref_axis',(1.,0.,0.));
#7428=DIRECTION('',(0.,0.,1.));
#7429=DIRECTION('center_axis',(0.,0.,-1.));
#7430=DIRECTION('ref_axis',(1.,0.,0.));
#7431=DIRECTION('center_axis',(0.,0.,1.));
#7432=DIRECTION('ref_axis',(1.,0.,0.));
#7433=DIRECTION('center_axis',(0.,0.,1.));
#7434=DIRECTION('ref_axis',(1.,0.,0.));
#7435=DIRECTION('center_axis',(0.,0.,1.));
#7436=DIRECTION('ref_axis',(1.,0.,0.));
#7437=DIRECTION('',(0.,1.,0.));
#7438=DIRECTION('',(0.,-1.,0.));
#7439=DIRECTION('center_axis',(0.,0.,1.));
#7440=DIRECTION('ref_axis',(1.,0.,0.));
#7441=DIRECTION('center_axis',(0.,0.,1.));
#7442=DIRECTION('ref_axis',(1.,0.,0.));
#7443=DIRECTION('',(0.,0.,1.));
#7444=DIRECTION('center_axis',(0.,0.,1.));
#7445=DIRECTION('ref_axis',(1.,0.,0.));
#7446=DIRECTION('center_axis',(0.,0.,1.));
#7447=DIRECTION('ref_axis',(1.,0.,0.));
#7448=DIRECTION('',(0.,0.,1.));
#7449=DIRECTION('center_axis',(1.,0.,0.));
#7450=DIRECTION('ref_axis',(0.,0.,-1.));
#7451=DIRECTION('center_axis',(1.,0.,0.));
#7452=DIRECTION('ref_axis',(0.,0.,-1.));
#7453=DIRECTION('',(1.,0.,0.));
#7454=DIRECTION('',(1.,0.,0.));
#7455=DIRECTION('center_axis',(-1.,0.,0.));
#7456=DIRECTION('ref_axis',(0.,0.,-1.));
#7457=DIRECTION('center_axis',(1.,0.,0.));
#7458=DIRECTION('ref_axis',(0.,1.,0.));
#7459=DIRECTION('',(0.,-1.,0.));
#7460=DIRECTION('center_axis',(-1.,0.,0.));
#7461=DIRECTION('ref_axis',(0.,-1.,0.));
#7462=DIRECTION('',(0.,-1.,0.));
#7463=DIRECTION('center_axis',(0.,0.,1.));
#7464=DIRECTION('ref_axis',(1.,0.,0.));
#7465=DIRECTION('axis',(0.,0.,1.));
#7466=DIRECTION('refdir',(1.,0.,0.));
#7467=DIRECTION('center_axis',(0.866025403784439,0.,-0.5));
#7468=DIRECTION('ref_axis',(0.5,0.,0.866025403784439));
#7469=DIRECTION('',(0.5,0.,0.866025403784439));
#7470=DIRECTION('',(0.,-1.,0.));
#7471=DIRECTION('',(0.5,0.,0.866025403784439));
#7472=DIRECTION('',(0.,-1.,0.));
#7473=DIRECTION('center_axis',(1.20185167898973E-16,0.,-1.));
#7474=DIRECTION('ref_axis',(1.,0.,1.20185167898973E-16));
#7475=DIRECTION('',(1.,0.,1.20185167898973E-16));
#7476=DIRECTION('',(0.,-1.,0.));
#7477=DIRECTION('',(1.,0.,1.20185167898973E-16));
#7478=DIRECTION('center_axis',(-0.866025403784439,0.,-0.5));
#7479=DIRECTION('ref_axis',(0.5,0.,-0.866025403784439));
#7480=DIRECTION('',(0.5,0.,-0.866025403784439));
#7481=DIRECTION('',(0.,-1.,0.));
#7482=DIRECTION('',(0.5,0.,-0.866025403784439));
#7483=DIRECTION('center_axis',(-0.866025403784439,0.,0.5));
#7484=DIRECTION('ref_axis',(-0.5,0.,-0.866025403784439));
#7485=DIRECTION('',(-0.5,0.,-0.866025403784439));
#7486=DIRECTION('',(0.,-1.,0.));
#7487=DIRECTION('',(-0.5,0.,-0.866025403784439));
#7488=DIRECTION('center_axis',(-2.40370335797945E-16,0.,1.));
#7489=DIRECTION('ref_axis',(-1.,0.,-2.40370335797945E-16));
#7490=DIRECTION('',(-1.,0.,-2.40370335797945E-16));
#7491=DIRECTION('',(0.,-1.,0.));
#7492=DIRECTION('',(-1.,0.,-2.40370335797945E-16));
#7493=DIRECTION('center_axis',(0.866025403784439,0.,0.5));
#7494=DIRECTION('ref_axis',(-0.5,0.,0.866025403784439));
#7495=DIRECTION('',(-0.5,0.,0.866025403784439));
#7496=DIRECTION('',(-0.5,0.,0.866025403784439));
#7497=DIRECTION('center_axis',(0.,-1.,0.));
#7498=DIRECTION('ref_axis',(0.,0.,-1.));
#7499=DIRECTION('center_axis',(0.,1.,0.));
#7500=DIRECTION('ref_axis',(0.,0.,1.));
#7501=DIRECTION('center_axis',(0.,-1.,0.));
#7502=DIRECTION('ref_axis',(1.,0.,0.));
#7503=DIRECTION('center_axis',(0.,-1.,0.));
#7504=DIRECTION('ref_axis',(1.,0.,0.));
#7505=DIRECTION('center_axis',(0.,-1.,0.));
#7506=DIRECTION('ref_axis',(1.,0.,0.));
#7507=DIRECTION('',(0.707106781186548,0.707106781186547,8.65956056235494E-17));
#7508=DIRECTION('center_axis',(0.,-1.,0.));
#7509=DIRECTION('ref_axis',(1.,0.,0.));
#7510=DIRECTION('center_axis',(0.,1.,0.));
#7511=DIRECTION('ref_axis',(1.,0.,0.));
#7512=DIRECTION('',(0.,1.,0.));
#7513=DIRECTION('center_axis',(0.,1.,0.));
#7514=DIRECTION('ref_axis',(1.,0.,0.));
#7515=DIRECTION('center_axis',(0.,-1.,0.));
#7516=DIRECTION('ref_axis',(1.,0.,0.));
#7517=DIRECTION('',(-0.707106781186548,0.707106781186547,-8.65956056235494E-17));
#7518=DIRECTION('center_axis',(0.,-1.,0.));
#7519=DIRECTION('ref_axis',(0.,0.,-1.));
#7520=DIRECTION('axis',(0.,0.,1.));
#7521=DIRECTION('refdir',(1.,0.,0.));
#7522=DIRECTION('axis',(0.,0.,1.));
#7523=DIRECTION('refdir',(1.,0.,0.));
#7524=DIRECTION('center_axis',(0.,0.,1.));
#7525=DIRECTION('ref_axis',(1.,0.,0.));
#7526=DIRECTION('center_axis',(0.,0.,1.));
#7527=DIRECTION('ref_axis',(1.,0.,0.));
#7528=DIRECTION('',(0.,0.,1.));
#7529=DIRECTION('center_axis',(0.,0.,-1.));
#7530=DIRECTION('ref_axis',(1.,0.,0.));
#7531=DIRECTION('center_axis',(0.,0.,1.));
#7532=DIRECTION('ref_axis',(1.,0.,0.));
#7533=DIRECTION('center_axis',(0.,0.,1.));
#7534=DIRECTION('ref_axis',(1.,0.,0.));
#7535=DIRECTION('',(0.,0.,1.));
#7536=DIRECTION('center_axis',(0.,0.,-1.));
#7537=DIRECTION('ref_axis',(1.,0.,0.));
#7538=DIRECTION('center_axis',(0.,0.,1.));
#7539=DIRECTION('ref_axis',(1.,0.,0.));
#7540=DIRECTION('center_axis',(0.,0.,1.));
#7541=DIRECTION('ref_axis',(1.,0.,0.));
#7542=DIRECTION('',(0.,0.,1.));
#7543=DIRECTION('center_axis',(0.,0.,-1.));
#7544=DIRECTION('ref_axis',(1.,0.,0.));
#7545=DIRECTION('center_axis',(0.,0.,1.));
#7546=DIRECTION('ref_axis',(-0.707106781186548,-0.707106781186547,0.));
#7547=DIRECTION('',(0.,0.,1.));
#7548=DIRECTION('center_axis',(0.,0.,1.));
#7549=DIRECTION('ref_axis',(1.,0.,0.));
#7550=DIRECTION('',(0.,0.,-1.));
#7551=DIRECTION('center_axis',(0.,0.,1.));
#7552=DIRECTION('ref_axis',(1.,0.,0.));
#7553=DIRECTION('center_axis',(-0.707106781186548,0.707106781186548,0.));
#7554=DIRECTION('ref_axis',(-0.707106781186548,-0.707106781186548,0.));
#7555=DIRECTION('',(-0.707106781186548,-0.707106781186548,0.));
#7556=DIRECTION('',(0.,0.,1.));
#7557=DIRECTION('',(0.707106781186548,0.707106781186548,0.));
#7558=DIRECTION('center_axis',(0.,0.,1.));
#7559=DIRECTION('ref_axis',(1.,0.,0.));
#7560=DIRECTION('',(0.707106781186548,0.707106781186548,0.));
#7561=DIRECTION('center_axis',(0.,0.,1.));
#7562=DIRECTION('ref_axis',(1.,0.,0.));
#7563=DIRECTION('',(1.,0.,0.));
#7564=DIRECTION('center_axis',(0.,0.,1.));
#7565=DIRECTION('ref_axis',(1.,0.,0.));
#7566=DIRECTION('',(-1.,0.,0.));
#7567=DIRECTION('center_axis',(0.,0.,1.));
#7568=DIRECTION('ref_axis',(1.,0.,0.));
#7569=DIRECTION('',(0.,1.,0.));
#7570=DIRECTION('center_axis',(0.,0.,1.));
#7571=DIRECTION('ref_axis',(1.,0.,0.));
#7572=DIRECTION('',(0.,-1.,0.));
#7573=DIRECTION('center_axis',(0.,0.,1.));
#7574=DIRECTION('ref_axis',(1.,0.,0.));
#7575=DIRECTION('center_axis',(0.707106781186548,-0.707106781186548,0.));
#7576=DIRECTION('ref_axis',(0.707106781186548,0.707106781186548,0.));
#7577=DIRECTION('',(-0.707106781186548,-0.707106781186548,0.));
#7578=DIRECTION('',(0.,0.,-1.));
#7579=DIRECTION('center_axis',(0.,0.,1.));
#7580=DIRECTION('ref_axis',(-0.923879532511287,0.38268343236509,0.));
#7581=DIRECTION('',(0.,0.,-1.));
#7582=DIRECTION('center_axis',(0.,0.,1.));
#7583=DIRECTION('ref_axis',(1.,0.,0.));
#7584=DIRECTION('center_axis',(0.,0.,1.));
#7585=DIRECTION('ref_axis',(1.,0.,0.));
#7586=DIRECTION('center_axis',(0.,0.,1.));
#7587=DIRECTION('ref_axis',(1.,0.,0.));
#7588=DIRECTION('',(0.,0.,1.));
#7589=DIRECTION('center_axis',(0.,0.,1.));
#7590=DIRECTION('ref_axis',(1.,0.,0.));
#7591=DIRECTION('',(0.,0.,-1.));
#7592=DIRECTION('',(0.,0.,1.));
#7593=DIRECTION('center_axis',(0.,0.,1.));
#7594=DIRECTION('ref_axis',(1.,0.,0.));
#7595=DIRECTION('center_axis',(0.,1.,0.));
#7596=DIRECTION('ref_axis',(-1.,0.,0.));
#7597=DIRECTION('',(1.,0.,0.));
#7598=DIRECTION('',(0.,0.,-1.));
#7599=DIRECTION('center_axis',(0.,0.,1.));
#7600=DIRECTION('ref_axis',(1.,0.,0.));
#7601=DIRECTION('',(0.,1.,0.));
#7602=DIRECTION('center_axis',(0.,0.,1.));
#7603=DIRECTION('ref_axis',(1.,0.,0.));
#7604=DIRECTION('',(0.,-1.,0.));
#7605=DIRECTION('center_axis',(0.,0.,1.));
#7606=DIRECTION('ref_axis',(1.,0.,0.));
#7607=DIRECTION('',(-1.,0.,0.));
#7608=DIRECTION('center_axis',(0.,0.,1.));
#7609=DIRECTION('ref_axis',(1.,0.,0.));
#7610=DIRECTION('center_axis',(0.,-1.,0.));
#7611=DIRECTION('ref_axis',(1.,0.,0.));
#7612=DIRECTION('center_axis',(0.,0.,1.));
#7613=DIRECTION('ref_axis',(6.12323399573677E-17,1.,0.));
#7614=DIRECTION('',(0.,0.,1.));
#7615=DIRECTION('',(0.,0.,-1.));
#7616=DIRECTION('center_axis',(1.,0.,0.));
#7617=DIRECTION('ref_axis',(0.,1.,0.));
#7618=DIRECTION('',(0.,0.,1.));
#7619=DIRECTION('center_axis',(-1.,0.,0.));
#7620=DIRECTION('ref_axis',(0.,-1.,0.));
#7621=DIRECTION('center_axis',(0.,0.,1.));
#7622=DIRECTION('ref_axis',(1.,0.,0.));
#7623=DIRECTION('center_axis',(0.,0.,1.));
#7624=DIRECTION('ref_axis',(1.,0.,0.));
#7625=DIRECTION('center_axis',(0.,0.,1.));
#7626=DIRECTION('ref_axis',(1.,0.,0.));
#7627=DIRECTION('center_axis',(0.,0.,-1.));
#7628=DIRECTION('ref_axis',(1.,0.,0.));
#7629=DIRECTION('center_axis',(0.,0.,1.));
#7630=DIRECTION('ref_axis',(1.,0.,0.));
#7631=DIRECTION('',(0.,0.,-1.));
#7632=DIRECTION('center_axis',(0.,0.,1.));
#7633=DIRECTION('ref_axis',(1.,0.,0.));
#7634=DIRECTION('',(0.,0.,-1.));
#7635=DIRECTION('center_axis',(0.,0.,1.));
#7636=DIRECTION('ref_axis',(1.,0.,0.));
#7637=DIRECTION('center_axis',(0.,0.,1.));
#7638=DIRECTION('ref_axis',(1.,0.,0.));
#7639=DIRECTION('axis',(0.,0.,1.));
#7640=DIRECTION('refdir',(1.,0.,0.));
#7641=DIRECTION('center_axis',(0.,0.,1.));
#7642=DIRECTION('ref_axis',(1.,0.,0.));
#7643=DIRECTION('center_axis',(0.,0.,1.));
#7644=DIRECTION('ref_axis',(1.,0.,0.));
#7645=DIRECTION('',(0.,0.,1.));
#7646=DIRECTION('center_axis',(0.,0.,1.));
#7647=DIRECTION('ref_axis',(1.,0.,0.));
#7648=DIRECTION('center_axis',(0.,0.,1.));
#7649=DIRECTION('ref_axis',(1.,0.,0.));
#7650=DIRECTION('center_axis',(0.,0.,1.));
#7651=DIRECTION('ref_axis',(1.,0.,0.));
#7652=DIRECTION('center_axis',(0.,0.,1.));
#7653=DIRECTION('ref_axis',(1.,0.,0.));
#7654=DIRECTION('',(0.,0.,-1.));
#7655=DIRECTION('center_axis',(0.,0.,1.));
#7656=DIRECTION('ref_axis',(1.,0.,0.));
#7657=DIRECTION('center_axis',(0.,0.,1.));
#7658=DIRECTION('ref_axis',(1.,0.,0.));
#7659=DIRECTION('center_axis',(0.,0.,1.));
#7660=DIRECTION('ref_axis',(1.,0.,0.));
#7661=DIRECTION('axis',(0.,0.,1.));
#7662=DIRECTION('refdir',(1.,0.,0.));
#7663=DIRECTION('center_axis',(0.,0.,1.));
#7664=DIRECTION('ref_axis',(1.,0.,0.));
#7665=DIRECTION('center_axis',(0.,0.,-1.));
#7666=DIRECTION('ref_axis',(1.,0.,0.));
#7667=DIRECTION('',(0.,0.,-1.));
#7668=DIRECTION('center_axis',(0.,0.,-1.));
#7669=DIRECTION('ref_axis',(1.,0.,0.));
#7670=DIRECTION('center_axis',(0.,0.,1.));
#7671=DIRECTION('ref_axis',(1.,0.,0.));
#7672=DIRECTION('center_axis',(0.,0.,1.));
#7673=DIRECTION('ref_axis',(1.,0.,0.));
#7674=DIRECTION('',(0.,0.,-1.));
#7675=DIRECTION('center_axis',(0.,0.,1.));
#7676=DIRECTION('ref_axis',(1.,0.,0.));
#7677=DIRECTION('center_axis',(0.,0.,1.));
#7678=DIRECTION('ref_axis',(1.,0.,0.));
#7679=DIRECTION('center_axis',(0.,0.,1.));
#7680=DIRECTION('ref_axis',(1.,0.,0.));
#7681=DIRECTION('axis',(0.,0.,1.));
#7682=DIRECTION('refdir',(1.,0.,0.));
#7683=DIRECTION('center_axis',(1.,0.,0.));
#7684=DIRECTION('ref_axis',(0.,0.,-1.));
#7685=DIRECTION('',(0.,0.,1.));
#7686=DIRECTION('center_axis',(1.,0.,0.));
#7687=DIRECTION('ref_axis',(0.,0.,-1.));
#7688=DIRECTION('center_axis',(1.,0.,0.));
#7689=DIRECTION('ref_axis',(0.,0.,-1.));
#7690=DIRECTION('center_axis',(1.,0.,0.));
#7691=DIRECTION('ref_axis',(0.,0.,-1.));
#7692=DIRECTION('',(1.,0.,0.));
#7693=DIRECTION('center_axis',(1.,0.,0.));
#7694=DIRECTION('ref_axis',(0.,0.,-1.));
#7695=DIRECTION('',(0.,0.,-1.));
#7696=DIRECTION('center_axis',(0.,0.,1.));
#7697=DIRECTION('ref_axis',(1.,0.,0.));
#7698=DIRECTION('center_axis',(0.,0.,-1.));
#7699=DIRECTION('ref_axis',(1.,0.,0.));
#7700=DIRECTION('',(0.,0.,-1.));
#7701=DIRECTION('center_axis',(0.,0.,-1.));
#7702=DIRECTION('ref_axis',(1.,0.,0.));
#7703=DIRECTION('center_axis',(0.,0.,1.));
#7704=DIRECTION('ref_axis',(1.,0.,0.));
#7705=DIRECTION('center_axis',(0.,0.,1.));
#7706=DIRECTION('ref_axis',(1.,0.,0.));
#7707=DIRECTION('',(0.,0.,-1.));
#7708=DIRECTION('center_axis',(0.,0.,1.));
#7709=DIRECTION('ref_axis',(1.,0.,0.));
#7710=DIRECTION('center_axis',(0.,0.,1.));
#7711=DIRECTION('ref_axis',(1.,0.,0.));
#7712=DIRECTION('center_axis',(0.,0.,1.));
#7713=DIRECTION('ref_axis',(1.,0.,0.));
#7714=DIRECTION('axis',(0.,0.,1.));
#7715=DIRECTION('refdir',(1.,0.,0.));
#7716=DIRECTION('center_axis',(0.,1.,0.));
#7717=DIRECTION('ref_axis',(0.,0.,1.));
#7718=DIRECTION('center_axis',(0.,-1.,0.));
#7719=DIRECTION('ref_axis',(1.,0.,0.));
#7720=DIRECTION('center_axis',(0.,-1.,0.));
#7721=DIRECTION('ref_axis',(1.,0.,0.));
#7722=DIRECTION('center_axis',(0.,-1.,0.));
#7723=DIRECTION('ref_axis',(1.,0.,0.));
#7724=DIRECTION('',(0.707106781186547,0.707106781186548,8.65956056235493E-17));
#7725=DIRECTION('center_axis',(0.,-1.,0.));
#7726=DIRECTION('ref_axis',(1.,0.,0.));
#7727=DIRECTION('center_axis',(0.,-1.,0.));
#7728=DIRECTION('ref_axis',(1.,0.,0.));
#7729=DIRECTION('',(0.,1.,0.));
#7730=DIRECTION('center_axis',(0.,1.,0.));
#7731=DIRECTION('ref_axis',(1.,0.,0.));
#7732=DIRECTION('center_axis',(0.,-1.,0.));
#7733=DIRECTION('ref_axis',(1.,0.,0.));
#7734=DIRECTION('',(-0.707106781186547,0.707106781186548,-8.65956056235493E-17));
#7735=DIRECTION('center_axis',(0.,-1.,0.));
#7736=DIRECTION('ref_axis',(0.,0.,-1.));
#7737=DIRECTION('center_axis',(0.,-1.,0.));
#7738=DIRECTION('ref_axis',(1.,0.,0.));
#7739=DIRECTION('center_axis',(0.,1.,0.));
#7740=DIRECTION('ref_axis',(1.,0.,0.));
#7741=DIRECTION('center_axis',(0.,1.,0.));
#7742=DIRECTION('ref_axis',(1.,0.,0.));
#7743=DIRECTION('',(-0.447213595499958,0.894427190999916,-5.47678698264203E-17));
#7744=DIRECTION('center_axis',(0.,-1.,0.));
#7745=DIRECTION('ref_axis',(1.,0.,0.));
#7746=DIRECTION('center_axis',(0.,1.,0.));
#7747=DIRECTION('ref_axis',(1.,0.,0.));
#7748=DIRECTION('',(0.,1.,0.));
#7749=DIRECTION('center_axis',(0.,1.,0.));
#7750=DIRECTION('ref_axis',(1.,0.,0.));
#7751=DIRECTION('center_axis',(0.,-1.,0.));
#7752=DIRECTION('ref_axis',(1.,0.,0.));
#7753=DIRECTION('',(-0.707106781186547,0.707106781186548,-8.65956056235493E-17));
#7754=DIRECTION('center_axis',(0.,-1.,0.));
#7755=DIRECTION('ref_axis',(0.,0.,-1.));
#7756=DIRECTION('center_axis',(0.866025403784439,0.,-0.5));
#7757=DIRECTION('ref_axis',(0.5,0.,0.866025403784439));
#7758=DIRECTION('',(-0.5,0.,-0.866025403784439));
#7759=DIRECTION('',(0.,-1.,0.));
#7760=DIRECTION('',(0.5,0.,0.866025403784439));
#7761=DIRECTION('',(0.,-1.,0.));
#7762=DIRECTION('center_axis',(1.60246890531964E-16,0.,-1.));
#7763=DIRECTION('ref_axis',(1.,0.,1.60246890531964E-16));
#7764=DIRECTION('',(-1.,0.,-1.60246890531964E-16));
#7765=DIRECTION('',(0.,-1.,0.));
#7766=DIRECTION('',(1.,0.,1.60246890531964E-16));
#7767=DIRECTION('center_axis',(-0.866025403784439,0.,-0.5));
#7768=DIRECTION('ref_axis',(0.5,0.,-0.866025403784439));
#7769=DIRECTION('',(-0.5,0.,0.866025403784439));
#7770=DIRECTION('',(0.,-1.,0.));
#7771=DIRECTION('',(0.5,0.,-0.866025403784439));
#7772=DIRECTION('center_axis',(-0.866025403784439,0.,0.5));
#7773=DIRECTION('ref_axis',(-0.5,0.,-0.866025403784439));
#7774=DIRECTION('',(0.5,0.,0.866025403784439));
#7775=DIRECTION('',(0.,-1.,0.));
#7776=DIRECTION('',(-0.5,0.,-0.866025403784439));
#7777=DIRECTION('center_axis',(-1.60246890531964E-16,0.,1.));
#7778=DIRECTION('ref_axis',(-1.,0.,-1.60246890531964E-16));
#7779=DIRECTION('',(1.,0.,1.60246890531964E-16));
#7780=DIRECTION('',(0.,-1.,0.));
#7781=DIRECTION('',(-1.,0.,-1.60246890531964E-16));
#7782=DIRECTION('center_axis',(0.866025403784439,0.,0.5));
#7783=DIRECTION('ref_axis',(-0.5,0.,0.866025403784439));
#7784=DIRECTION('',(0.5,0.,-0.866025403784439));
#7785=DIRECTION('',(-0.5,0.,0.866025403784439));
#7786=DIRECTION('center_axis',(0.,1.,0.));
#7787=DIRECTION('ref_axis',(1.,0.,0.));
#7788=DIRECTION('center_axis',(0.,-1.,0.));
#7789=DIRECTION('ref_axis',(0.,0.,-1.));
#7790=DIRECTION('axis',(0.,0.,1.));
#7791=DIRECTION('refdir',(1.,0.,0.));
#7792=DIRECTION('center_axis',(0.,1.,0.));
#7793=DIRECTION('ref_axis',(1.,0.,0.));
#7794=DIRECTION('center_axis',(0.,1.,0.));
#7795=DIRECTION('ref_axis',(1.,0.,0.));
#7796=DIRECTION('center_axis',(0.866025403784439,0.,-0.5));
#7797=DIRECTION('ref_axis',(0.5,0.,0.866025403784439));
#7798=DIRECTION('',(0.5,0.,0.866025403784439));
#7799=DIRECTION('',(0.,-1.,0.));
#7800=DIRECTION('',(0.5,0.,0.866025403784439));
#7801=DIRECTION('',(0.,-1.,0.));
#7802=DIRECTION('center_axis',(1.20185167898973E-16,0.,-1.));
#7803=DIRECTION('ref_axis',(1.,0.,1.20185167898973E-16));
#7804=DIRECTION('',(1.,0.,1.20185167898973E-16));
#7805=DIRECTION('',(0.,-1.,0.));
#7806=DIRECTION('',(1.,0.,1.20185167898973E-16));
#7807=DIRECTION('center_axis',(-0.866025403784439,0.,-0.5));
#7808=DIRECTION('ref_axis',(0.5,0.,-0.866025403784439));
#7809=DIRECTION('',(0.5,0.,-0.866025403784439));
#7810=DIRECTION('',(0.,-1.,0.));
#7811=DIRECTION('',(0.5,0.,-0.866025403784439));
#7812=DIRECTION('center_axis',(-0.866025403784439,0.,0.5));
#7813=DIRECTION('ref_axis',(-0.5,0.,-0.866025403784439));
#7814=DIRECTION('',(-0.5,0.,-0.866025403784439));
#7815=DIRECTION('',(0.,-1.,0.));
#7816=DIRECTION('',(-0.5,0.,-0.866025403784439));
#7817=DIRECTION('center_axis',(-2.40370335797945E-16,0.,1.));
#7818=DIRECTION('ref_axis',(-1.,0.,-2.40370335797945E-16));
#7819=DIRECTION('',(-1.,0.,-2.40370335797945E-16));
#7820=DIRECTION('',(0.,-1.,0.));
#7821=DIRECTION('',(-1.,0.,-2.40370335797945E-16));
#7822=DIRECTION('center_axis',(0.866025403784439,0.,0.5));
#7823=DIRECTION('ref_axis',(-0.5,0.,0.866025403784439));
#7824=DIRECTION('',(-0.5,0.,0.866025403784439));
#7825=DIRECTION('',(-0.5,0.,0.866025403784439));
#7826=DIRECTION('center_axis',(0.,-1.,0.));
#7827=DIRECTION('ref_axis',(0.,0.,-1.));
#7828=DIRECTION('center_axis',(0.,1.,0.));
#7829=DIRECTION('ref_axis',(0.,0.,1.));
#7830=DIRECTION('center_axis',(0.,-1.,0.));
#7831=DIRECTION('ref_axis',(1.,0.,0.));
#7832=DIRECTION('center_axis',(0.,-1.,0.));
#7833=DIRECTION('ref_axis',(1.,0.,0.));
#7834=DIRECTION('center_axis',(0.,-1.,0.));
#7835=DIRECTION('ref_axis',(1.,0.,0.));
#7836=DIRECTION('',(0.707106781186548,0.707106781186547,8.65956056235494E-17));
#7837=DIRECTION('center_axis',(0.,-1.,0.));
#7838=DIRECTION('ref_axis',(1.,0.,0.));
#7839=DIRECTION('',(0.,1.,0.));
#7840=DIRECTION('axis',(0.,0.,1.));
#7841=DIRECTION('refdir',(1.,0.,0.));
#7842=DIRECTION('center_axis',(0.,0.,1.));
#7843=DIRECTION('ref_axis',(1.,0.,0.));
#7844=DIRECTION('center_axis',(0.,0.,1.));
#7845=DIRECTION('ref_axis',(1.,0.,0.));
#7846=DIRECTION('',(0.,0.,1.));
#7847=DIRECTION('center_axis',(0.,0.,-1.));
#7848=DIRECTION('ref_axis',(1.,0.,0.));
#7849=DIRECTION('center_axis',(0.,0.,1.));
#7850=DIRECTION('ref_axis',(1.,0.,0.));
#7851=DIRECTION('center_axis',(0.,0.,1.));
#7852=DIRECTION('ref_axis',(1.,0.,0.));
#7853=DIRECTION('center_axis',(0.,0.,1.));
#7854=DIRECTION('ref_axis',(1.,0.,0.));
#7855=DIRECTION('center_axis',(0.,0.,1.));
#7856=DIRECTION('ref_axis',(1.,0.,0.));
#7857=DIRECTION('center_axis',(0.,0.,1.));
#7858=DIRECTION('ref_axis',(1.,0.,0.));
#7859=DIRECTION('center_axis',(0.,0.,1.));
#7860=DIRECTION('ref_axis',(1.,0.,0.));
#7861=DIRECTION('center_axis',(0.,0.,-1.));
#7862=DIRECTION('ref_axis',(1.,0.,0.));
#7863=DIRECTION('center_axis',(0.,0.,1.));
#7864=DIRECTION('ref_axis',(1.,0.,0.));
#7865=DIRECTION('',(0.,0.,-1.));
#7866=DIRECTION('center_axis',(0.,0.,1.));
#7867=DIRECTION('ref_axis',(1.,0.,0.));
#7868=DIRECTION('',(0.,0.,-1.));
#7869=DIRECTION('center_axis',(0.,0.,1.));
#7870=DIRECTION('ref_axis',(1.,0.,0.));
#7871=DIRECTION('center_axis',(0.,0.,1.));
#7872=DIRECTION('ref_axis',(1.,0.,0.));
#7873=DIRECTION('center_axis',(0.,0.,1.));
#7874=DIRECTION('ref_axis',(1.,0.,0.));
#7875=DIRECTION('',(0.,0.,-1.));
#7876=DIRECTION('center_axis',(0.,0.,1.));
#7877=DIRECTION('ref_axis',(1.,0.,0.));
#7878=DIRECTION('center_axis',(0.,0.,1.));
#7879=DIRECTION('ref_axis',(1.,0.,0.));
#7880=DIRECTION('axis',(0.,0.,1.));
#7881=DIRECTION('refdir',(1.,0.,0.));
#7882=DIRECTION('center_axis',(0.,0.,1.));
#7883=DIRECTION('ref_axis',(1.,0.,0.));
#7884=DIRECTION('center_axis',(0.,0.,-1.));
#7885=DIRECTION('ref_axis',(1.,0.,0.));
#7886=DIRECTION('',(0.,0.,-1.));
#7887=DIRECTION('center_axis',(0.,0.,-1.));
#7888=DIRECTION('ref_axis',(1.,0.,0.));
#7889=DIRECTION('center_axis',(0.,0.,1.));
#7890=DIRECTION('ref_axis',(1.,0.,0.));
#7891=DIRECTION('center_axis',(0.,0.,1.));
#7892=DIRECTION('ref_axis',(1.,0.,0.));
#7893=DIRECTION('',(0.,0.,-1.));
#7894=DIRECTION('center_axis',(0.,0.,1.));
#7895=DIRECTION('ref_axis',(1.,0.,0.));
#7896=DIRECTION('center_axis',(0.,0.,1.));
#7897=DIRECTION('ref_axis',(1.,0.,0.));
#7898=DIRECTION('center_axis',(0.,0.,1.));
#7899=DIRECTION('ref_axis',(1.,0.,0.));
#7900=DIRECTION('axis',(0.,0.,1.));
#7901=DIRECTION('refdir',(1.,0.,0.));
#7902=DIRECTION('axis',(0.,0.,1.));
#7903=DIRECTION('refdir',(1.,0.,0.));
#7904=DIRECTION('center_axis',(0.,0.,1.));
#7905=DIRECTION('ref_axis',(1.,0.,0.));
#7906=DIRECTION('center_axis',(0.,0.,1.));
#7907=DIRECTION('ref_axis',(1.,0.,0.));
#7908=DIRECTION('',(0.,0.,1.));
#7909=DIRECTION('center_axis',(0.,0.,-1.));
#7910=DIRECTION('ref_axis',(1.,0.,0.));
#7911=DIRECTION('center_axis',(0.,0.,1.));
#7912=DIRECTION('ref_axis',(1.,0.,0.));
#7913=DIRECTION('center_axis',(0.,0.,1.));
#7914=DIRECTION('ref_axis',(1.,0.,0.));
#7915=DIRECTION('',(0.,0.,1.));
#7916=DIRECTION('center_axis',(0.,0.,-1.));
#7917=DIRECTION('ref_axis',(1.,0.,0.));
#7918=DIRECTION('center_axis',(0.,0.,1.));
#7919=DIRECTION('ref_axis',(1.,0.,0.));
#7920=DIRECTION('',(0.,0.,-1.));
#7921=DIRECTION('center_axis',(0.,0.,1.));
#7922=DIRECTION('ref_axis',(1.,0.,0.));
#7923=DIRECTION('',(0.,0.,1.));
#7924=DIRECTION('center_axis',(0.,0.,1.));
#7925=DIRECTION('ref_axis',(1.,0.,0.));
#7926=DIRECTION('center_axis',(-0.257662650560332,0.966234939601246,0.));
#7927=DIRECTION('ref_axis',(-0.966234939601246,-0.257662650560332,0.));
#7928=DIRECTION('',(0.966234939601246,0.257662650560332,0.));
#7929=DIRECTION('',(0.,0.,-1.));
#7930=DIRECTION('',(-0.966234939601246,-0.257662650560332,0.));
#7931=DIRECTION('center_axis',(0.,0.,1.));
#7932=DIRECTION('ref_axis',(1.,0.,0.));
#7933=DIRECTION('',(-0.966234939601246,-0.257662650560332,0.));
#7934=DIRECTION('center_axis',(0.,0.,1.));
#7935=DIRECTION('ref_axis',(1.,0.,0.));
#7936=DIRECTION('center_axis',(0.257662650560332,-0.966234939601246,0.));
#7937=DIRECTION('ref_axis',(0.966234939601246,0.257662650560332,0.));
#7938=DIRECTION('',(0.966234939601246,0.257662650560332,0.));
#7939=DIRECTION('',(0.,0.,1.));
#7940=DIRECTION('center_axis',(0.,0.,1.));
#7941=DIRECTION('ref_axis',(-0.966234939601246,-0.257662650560332,0.));
#7942=DIRECTION('center_axis',(0.,0.,1.));
#7943=DIRECTION('ref_axis',(1.,0.,0.));
#7944=DIRECTION('center_axis',(0.,0.,1.));
#7945=DIRECTION('ref_axis',(1.,0.,0.));
#7946=DIRECTION('axis',(0.,0.,1.));
#7947=DIRECTION('refdir',(1.,0.,0.));
#7948=DIRECTION('center_axis',(0.,0.,1.));
#7949=DIRECTION('ref_axis',(1.,0.,0.));
#7950=DIRECTION('center_axis',(0.,0.,-1.));
#7951=DIRECTION('ref_axis',(1.,0.,0.));
#7952=DIRECTION('',(0.,0.,-1.));
#7953=DIRECTION('center_axis',(0.,0.,-1.));
#7954=DIRECTION('ref_axis',(1.,0.,0.));
#7955=DIRECTION('center_axis',(0.,0.,1.));
#7956=DIRECTION('ref_axis',(1.,0.,0.));
#7957=DIRECTION('center_axis',(0.,0.,1.));
#7958=DIRECTION('ref_axis',(1.,0.,0.));
#7959=DIRECTION('',(0.,0.,-1.));
#7960=DIRECTION('center_axis',(0.,0.,1.));
#7961=DIRECTION('ref_axis',(1.,0.,0.));
#7962=DIRECTION('center_axis',(0.,0.,1.));
#7963=DIRECTION('ref_axis',(1.,0.,0.));
#7964=DIRECTION('center_axis',(0.,0.,1.));
#7965=DIRECTION('ref_axis',(1.,0.,0.));
#7966=DIRECTION('',(0.,0.,1.));
#7967=DIRECTION('',(1.,0.,0.));
#7968=DIRECTION('',(0.,0.,1.));
#7969=DIRECTION('',(1.,0.,0.));
#7970=DIRECTION('',(0.,0.,1.));
#7971=DIRECTION('',(1.,0.,0.));
#7972=DIRECTION('axis',(0.,0.,1.));
#7973=DIRECTION('refdir',(1.,0.,0.));
#7974=DIRECTION('axis',(0.,0.,1.));
#7975=DIRECTION('refdir',(1.,0.,0.));
#7976=DIRECTION('center_axis',(0.,0.,1.));
#7977=DIRECTION('ref_axis',(1.,0.,0.));
#7978=DIRECTION('center_axis',(0.,0.,1.));
#7979=DIRECTION('ref_axis',(1.,0.,0.));
#7980=DIRECTION('',(0.,0.,1.));
#7981=DIRECTION('center_axis',(0.,0.,-1.));
#7982=DIRECTION('ref_axis',(1.,0.,0.));
#7983=DIRECTION('center_axis',(0.,0.,1.));
#7984=DIRECTION('ref_axis',(1.,0.,0.));
#7985=DIRECTION('center_axis',(0.,0.,1.));
#7986=DIRECTION('ref_axis',(1.,0.,0.));
#7987=DIRECTION('center_axis',(0.,0.,1.));
#7988=DIRECTION('ref_axis',(1.,0.,0.));
#7989=DIRECTION('center_axis',(0.,0.,1.));
#7990=DIRECTION('ref_axis',(1.,0.,0.));
#7991=DIRECTION('center_axis',(0.,0.,1.));
#7992=DIRECTION('ref_axis',(1.,0.,0.));
#7993=DIRECTION('center_axis',(0.,0.,1.));
#7994=DIRECTION('ref_axis',(1.,0.,0.));
#7995=DIRECTION('center_axis',(0.,0.,-1.));
#7996=DIRECTION('ref_axis',(1.,0.,0.));
#7997=DIRECTION('center_axis',(0.,0.,1.));
#7998=DIRECTION('ref_axis',(1.,0.,0.));
#7999=DIRECTION('',(0.,0.,-1.));
#8000=DIRECTION('center_axis',(0.,0.,1.));
#8001=DIRECTION('ref_axis',(1.,0.,0.));
#8002=DIRECTION('',(0.,0.,-1.));
#8003=DIRECTION('center_axis',(0.,0.,1.));
#8004=DIRECTION('ref_axis',(1.,0.,0.));
#8005=DIRECTION('center_axis',(0.,0.,1.));
#8006=DIRECTION('ref_axis',(1.,0.,0.));
#8007=DIRECTION('center_axis',(0.,0.,1.));
#8008=DIRECTION('ref_axis',(1.,0.,0.));
#8009=DIRECTION('',(0.,0.,-1.));
#8010=DIRECTION('center_axis',(0.,0.,1.));
#8011=DIRECTION('ref_axis',(1.,0.,0.));
#8012=DIRECTION('center_axis',(0.,0.,1.));
#8013=DIRECTION('ref_axis',(1.,0.,0.));
#8014=DIRECTION('axis',(0.,0.,1.));
#8015=DIRECTION('refdir',(1.,0.,0.));
#8016=DIRECTION('center_axis',(0.,0.,1.));
#8017=DIRECTION('ref_axis',(1.,0.,0.));
#8018=DIRECTION('center_axis',(0.,0.,-1.));
#8019=DIRECTION('ref_axis',(1.,0.,0.));
#8020=DIRECTION('',(0.,0.,-1.));
#8021=DIRECTION('center_axis',(0.,0.,-1.));
#8022=DIRECTION('ref_axis',(1.,0.,0.));
#8023=DIRECTION('center_axis',(0.,0.,1.));
#8024=DIRECTION('ref_axis',(1.,0.,0.));
#8025=DIRECTION('center_axis',(0.,0.,1.));
#8026=DIRECTION('ref_axis',(1.,0.,0.));
#8027=DIRECTION('',(0.,0.,-1.));
#8028=DIRECTION('center_axis',(0.,0.,1.));
#8029=DIRECTION('ref_axis',(1.,0.,0.));
#8030=DIRECTION('center_axis',(0.,0.,1.));
#8031=DIRECTION('ref_axis',(1.,0.,0.));
#8032=DIRECTION('center_axis',(0.,0.,1.));
#8033=DIRECTION('ref_axis',(1.,0.,0.));
#8034=DIRECTION('axis',(0.,0.,1.));
#8035=DIRECTION('refdir',(1.,0.,0.));
#8036=DIRECTION('center_axis',(0.,0.,1.));
#8037=DIRECTION('ref_axis',(1.,0.,0.));
#8038=DIRECTION('center_axis',(0.,0.,1.));
#8039=DIRECTION('ref_axis',(1.,0.,0.));
#8040=DIRECTION('',(0.,0.,1.));
#8041=DIRECTION('center_axis',(0.,0.,-1.));
#8042=DIRECTION('ref_axis',(1.,0.,0.));
#8043=DIRECTION('center_axis',(0.,0.,1.));
#8044=DIRECTION('ref_axis',(1.,0.,0.));
#8045=DIRECTION('center_axis',(1.,0.,0.));
#8046=DIRECTION('ref_axis',(0.,0.,-1.));
#8047=DIRECTION('center_axis',(1.,0.,0.));
#8048=DIRECTION('ref_axis',(0.,0.,-1.));
#8049=DIRECTION('',(1.,0.,0.));
#8050=DIRECTION('center_axis',(-1.,0.,0.));
#8051=DIRECTION('ref_axis',(0.,0.,-1.));
#8052=DIRECTION('center_axis',(1.,0.,0.));
#8053=DIRECTION('ref_axis',(0.,0.,-1.));
#8054=DIRECTION('center_axis',(1.,0.,0.));
#8055=DIRECTION('ref_axis',(0.,0.,-1.));
#8056=DIRECTION('',(1.,0.,0.));
#8057=DIRECTION('center_axis',(-1.,0.,0.));
#8058=DIRECTION('ref_axis',(0.,0.,-1.));
#8059=DIRECTION('center_axis',(1.,0.,0.));
#8060=DIRECTION('ref_axis',(0.,0.,-1.));
#8061=DIRECTION('center_axis',(1.,0.,0.));
#8062=DIRECTION('ref_axis',(0.,0.,-1.));
#8063=DIRECTION('',(1.,0.,0.));
#8064=DIRECTION('center_axis',(-1.,0.,0.));
#8065=DIRECTION('ref_axis',(0.,0.,-1.));
#8066=DIRECTION('center_axis',(1.,0.,0.));
#8067=DIRECTION('ref_axis',(0.,0.,-1.));
#8068=DIRECTION('center_axis',(1.,0.,0.));
#8069=DIRECTION('ref_axis',(0.,0.,-1.));
#8070=DIRECTION('',(1.,0.,0.));
#8071=DIRECTION('center_axis',(-1.,0.,0.));
#8072=DIRECTION('ref_axis',(0.,0.,-1.));
#8073=DIRECTION('center_axis',(1.,0.,0.));
#8074=DIRECTION('ref_axis',(0.,0.,-1.));
#8075=DIRECTION('center_axis',(1.,0.,0.));
#8076=DIRECTION('ref_axis',(0.,0.,-1.));
#8077=DIRECTION('',(1.,0.,0.));
#8078=DIRECTION('center_axis',(-1.,0.,0.));
#8079=DIRECTION('ref_axis',(0.,0.,-1.));
#8080=DIRECTION('center_axis',(0.,1.,0.));
#8081=DIRECTION('ref_axis',(-1.,0.,0.));
#8082=DIRECTION('',(-1.,0.,0.));
#8083=DIRECTION('',(0.,0.,1.));
#8084=DIRECTION('',(-1.,0.,0.));
#8085=DIRECTION('',(0.,0.,1.));
#8086=DIRECTION('center_axis',(1.,0.,0.));
#8087=DIRECTION('ref_axis',(0.,1.,0.));
#8088=DIRECTION('',(0.,1.,0.));
#8089=DIRECTION('',(0.,1.,0.));
#8090=DIRECTION('',(0.,0.,1.));
#8091=DIRECTION('center_axis',(0.,-1.,0.));
#8092=DIRECTION('ref_axis',(1.,0.,0.));
#8093=DIRECTION('',(1.,0.,0.));
#8094=DIRECTION('',(1.,0.,0.));
#8095=DIRECTION('',(0.,0.,1.));
#8096=DIRECTION('center_axis',(-1.,0.,0.));
#8097=DIRECTION('ref_axis',(0.,-1.,0.));
#8098=DIRECTION('',(0.,-1.,0.));
#8099=DIRECTION('',(0.,-1.,0.));
#8100=DIRECTION('center_axis',(0.,0.,1.));
#8101=DIRECTION('ref_axis',(1.,0.,0.));
#8102=DIRECTION('center_axis',(0.,0.,1.));
#8103=DIRECTION('ref_axis',(1.,0.,0.));
#8104=DIRECTION('axis',(0.,0.,1.));
#8105=DIRECTION('refdir',(1.,0.,0.));
#8106=DIRECTION('axis',(0.,0.,1.));
#8107=DIRECTION('refdir',(1.,0.,0.));
#8108=DIRECTION('center_axis',(0.,1.,0.));
#8109=DIRECTION('ref_axis',(0.,0.,1.));
#8110=DIRECTION('center_axis',(0.,-1.,0.));
#8111=DIRECTION('ref_axis',(1.,0.,0.));
#8112=DIRECTION('',(-1.,0.,0.));
#8113=DIRECTION('',(0.,0.,-1.));
#8114=DIRECTION('',(1.,0.,0.));
#8115=DIRECTION('center_axis',(0.,0.,1.));
#8116=DIRECTION('ref_axis',(1.,0.,0.));
#8117=DIRECTION('',(0.,-1.,0.));
#8118=DIRECTION('',(0.,1.,0.));
#8119=DIRECTION('',(-1.,0.,0.));
#8120=DIRECTION('center_axis',(0.,-1.,0.));
#8121=DIRECTION('ref_axis',(0.,0.,-1.));
#8122=DIRECTION('center_axis',(0.,1.,0.));
#8123=DIRECTION('ref_axis',(1.,0.,0.));
#8124=DIRECTION('',(0.,0.,1.));
#8125=DIRECTION('',(1.,0.,0.));
#8126=DIRECTION('center_axis',(0.,0.,-1.));
#8127=DIRECTION('ref_axis',(-1.,0.,0.));
#8128=DIRECTION('',(0.,1.,0.));
#8129=DIRECTION('',(0.,1.,0.));
#8130=DIRECTION('center_axis',(1.,0.,0.));
#8131=DIRECTION('ref_axis',(0.,0.,-1.));
#8132=DIRECTION('center_axis',(0.,1.,0.));
#8133=DIRECTION('ref_axis',(0.,0.,1.));
#8134=DIRECTION('center_axis',(0.,-1.,0.));
#8135=DIRECTION('ref_axis',(1.,0.,0.));
#8136=DIRECTION('center_axis',(0.,-1.,0.));
#8137=DIRECTION('ref_axis',(1.,0.,0.));
#8138=DIRECTION('center_axis',(0.,-1.,0.));
#8139=DIRECTION('ref_axis',(1.,0.,0.));
#8140=DIRECTION('center_axis',(0.,-1.,0.));
#8141=DIRECTION('ref_axis',(1.,0.,0.));
#8142=DIRECTION('',(0.,1.,0.));
#8143=DIRECTION('center_axis',(0.,-1.,0.));
#8144=DIRECTION('ref_axis',(0.,0.,-1.));
#8145=DIRECTION('center_axis',(0.,-1.,0.));
#8146=DIRECTION('ref_axis',(1.,0.,0.));
#8147=DIRECTION('center_axis',(0.,-1.,0.));
#8148=DIRECTION('ref_axis',(1.,0.,0.));
#8149=DIRECTION('center_axis',(0.,-1.,0.));
#8150=DIRECTION('ref_axis',(1.,0.,0.));
#8151=DIRECTION('',(0.,1.,0.));
#8152=DIRECTION('center_axis',(0.,1.,0.));
#8153=DIRECTION('ref_axis',(0.,0.,1.));
#8154=DIRECTION('center_axis',(0.,-1.,0.));
#8155=DIRECTION('ref_axis',(1.,0.,0.));
#8156=DIRECTION('center_axis',(0.,-1.,0.));
#8157=DIRECTION('ref_axis',(1.,0.,0.));
#8158=DIRECTION('center_axis',(0.,-1.,0.));
#8159=DIRECTION('ref_axis',(1.,0.,0.));
#8160=DIRECTION('',(0.,1.,0.));
#8161=DIRECTION('center_axis',(0.,-1.,0.));
#8162=DIRECTION('ref_axis',(0.,0.,-1.));
#8163=DIRECTION('center_axis',(0.,-1.,0.));
#8164=DIRECTION('ref_axis',(1.,0.,0.));
#8165=DIRECTION('center_axis',(0.,-1.,0.));
#8166=DIRECTION('ref_axis',(1.,0.,0.));
#8167=DIRECTION('center_axis',(0.,-1.,0.));
#8168=DIRECTION('ref_axis',(1.,0.,0.));
#8169=DIRECTION('',(0.,1.,0.));
#8170=DIRECTION('center_axis',(0.,1.,0.));
#8171=DIRECTION('ref_axis',(0.,0.,1.));
#8172=DIRECTION('center_axis',(0.,-1.,0.));
#8173=DIRECTION('ref_axis',(1.,0.,0.));
#8174=DIRECTION('center_axis',(0.,-1.,0.));
#8175=DIRECTION('ref_axis',(1.,0.,0.));
#8176=DIRECTION('center_axis',(0.,-1.,0.));
#8177=DIRECTION('ref_axis',(1.,0.,0.));
#8178=DIRECTION('',(0.,1.,0.));
#8179=DIRECTION('center_axis',(0.,-1.,0.));
#8180=DIRECTION('ref_axis',(0.,0.,-1.));
#8181=DIRECTION('center_axis',(0.,-1.,0.));
#8182=DIRECTION('ref_axis',(1.,0.,0.));
#8183=DIRECTION('center_axis',(0.,-1.,0.));
#8184=DIRECTION('ref_axis',(1.,0.,0.));
#8185=DIRECTION('',(0.,1.,0.));
#8186=DIRECTION('axis',(0.,0.,1.));
#8187=DIRECTION('refdir',(1.,0.,0.));
#8188=DIRECTION('center_axis',(0.,1.,0.));
#8189=DIRECTION('ref_axis',(0.,0.,1.));
#8190=DIRECTION('center_axis',(0.,1.,0.));
#8191=DIRECTION('ref_axis',(1.,0.,0.));
#8192=DIRECTION('',(1.,0.,0.));
#8193=DIRECTION('center_axis',(0.,-1.,0.));
#8194=DIRECTION('ref_axis',(1.,0.,0.));
#8195=DIRECTION('',(-1.,0.,0.));
#8196=DIRECTION('center_axis',(0.,0.,-1.));
#8197=DIRECTION('ref_axis',(-1.,0.,0.));
#8198=DIRECTION('',(0.,-1.,0.));
#8199=DIRECTION('',(0.,1.,0.));
#8200=DIRECTION('',(1.,0.,0.));
#8201=DIRECTION('center_axis',(0.,-1.,0.));
#8202=DIRECTION('ref_axis',(0.,0.,-1.));
#8203=DIRECTION('center_axis',(0.,-1.,0.));
#8204=DIRECTION('ref_axis',(1.,0.,0.));
#8205=DIRECTION('center_axis',(0.,1.,0.));
#8206=DIRECTION('ref_axis',(1.,0.,0.));
#8207=DIRECTION('',(-1.,0.,0.));
#8208=DIRECTION('center_axis',(0.,0.,1.));
#8209=DIRECTION('ref_axis',(1.,0.,0.));
#8210=DIRECTION('',(0.,1.,0.));
#8211=DIRECTION('',(0.,-1.,0.));
#8212=DIRECTION('center_axis',(0.,1.,0.));
#8213=DIRECTION('ref_axis',(0.,0.,1.));
#8214=DIRECTION('center_axis',(0.,-1.,0.));
#8215=DIRECTION('ref_axis',(1.,0.,0.));
#8216=DIRECTION('center_axis',(0.,-1.,0.));
#8217=DIRECTION('ref_axis',(1.,0.,0.));
#8218=DIRECTION('center_axis',(0.,-1.,0.));
#8219=DIRECTION('ref_axis',(1.,0.,0.));
#8220=DIRECTION('center_axis',(0.,-1.,0.));
#8221=DIRECTION('ref_axis',(1.,0.,0.));
#8222=DIRECTION('',(0.,1.,0.));
#8223=DIRECTION('center_axis',(0.,-1.,0.));
#8224=DIRECTION('ref_axis',(0.,0.,-1.));
#8225=DIRECTION('center_axis',(0.,-1.,0.));
#8226=DIRECTION('ref_axis',(1.,0.,0.));
#8227=DIRECTION('center_axis',(0.,-1.,0.));
#8228=DIRECTION('ref_axis',(1.,0.,0.));
#8229=DIRECTION('',(0.,1.,0.));
#8230=DIRECTION('',(0.,0.,1.));
#8231=DIRECTION('',(1.,0.,0.));
#8232=DIRECTION('',(0.,0.,1.));
#8233=DIRECTION('',(1.,0.,0.));
#8234=DIRECTION('axis',(0.,0.,1.));
#8235=DIRECTION('refdir',(1.,0.,0.));
#8236=DIRECTION('center_axis',(1.,0.,0.));
#8237=DIRECTION('ref_axis',(0.,0.,-1.));
#8238=DIRECTION('center_axis',(1.,0.,0.));
#8239=DIRECTION('ref_axis',(0.,0.,-1.));
#8240=DIRECTION('',(1.,0.,0.));
#8241=DIRECTION('center_axis',(-1.,0.,0.));
#8242=DIRECTION('ref_axis',(0.,0.,-1.));
#8243=DIRECTION('center_axis',(1.,0.,0.));
#8244=DIRECTION('ref_axis',(0.,0.,-1.));
#8245=DIRECTION('center_axis',(1.,0.,0.));
#8246=DIRECTION('ref_axis',(0.,0.,-1.));
#8247=DIRECTION('',(1.,0.,0.));
#8248=DIRECTION('center_axis',(-1.,0.,0.));
#8249=DIRECTION('ref_axis',(0.,0.,-1.));
#8250=DIRECTION('center_axis',(1.,0.,0.));
#8251=DIRECTION('ref_axis',(0.,0.,-1.));
#8252=DIRECTION('center_axis',(1.,0.,0.));
#8253=DIRECTION('ref_axis',(0.,0.,-1.));
#8254=DIRECTION('',(1.,0.,0.));
#8255=DIRECTION('center_axis',(-1.,0.,0.));
#8256=DIRECTION('ref_axis',(0.,0.,-1.));
#8257=DIRECTION('center_axis',(1.,0.,0.));
#8258=DIRECTION('ref_axis',(0.,0.,-1.));
#8259=DIRECTION('center_axis',(1.,0.,0.));
#8260=DIRECTION('ref_axis',(0.,0.,-1.));
#8261=DIRECTION('',(1.,0.,0.));
#8262=DIRECTION('center_axis',(-1.,0.,0.));
#8263=DIRECTION('ref_axis',(0.,0.,-1.));
#8264=DIRECTION('center_axis',(1.,0.,0.));
#8265=DIRECTION('ref_axis',(0.,0.,-1.));
#8266=DIRECTION('center_axis',(1.,0.,0.));
#8267=DIRECTION('ref_axis',(0.,0.,-1.));
#8268=DIRECTION('',(1.,0.,0.));
#8269=DIRECTION('center_axis',(-1.,0.,0.));
#8270=DIRECTION('ref_axis',(0.,0.,-1.));
#8271=DIRECTION('center_axis',(0.,1.,0.));
#8272=DIRECTION('ref_axis',(-1.,0.,0.));
#8273=DIRECTION('',(-1.,0.,0.));
#8274=DIRECTION('',(0.,0.,1.));
#8275=DIRECTION('',(-1.,0.,0.));
#8276=DIRECTION('',(0.,0.,1.));
#8277=DIRECTION('center_axis',(1.,0.,0.));
#8278=DIRECTION('ref_axis',(0.,1.,0.));
#8279=DIRECTION('',(0.,1.,0.));
#8280=DIRECTION('',(0.,1.,0.));
#8281=DIRECTION('',(0.,0.,1.));
#8282=DIRECTION('center_axis',(0.,-1.,0.));
#8283=DIRECTION('ref_axis',(1.,0.,0.));
#8284=DIRECTION('',(1.,0.,0.));
#8285=DIRECTION('',(1.,0.,0.));
#8286=DIRECTION('',(0.,0.,1.));
#8287=DIRECTION('center_axis',(-1.,0.,0.));
#8288=DIRECTION('ref_axis',(0.,-1.,0.));
#8289=DIRECTION('',(0.,-1.,0.));
#8290=DIRECTION('',(0.,-1.,0.));
#8291=DIRECTION('center_axis',(0.,0.,1.));
#8292=DIRECTION('ref_axis',(1.,0.,0.));
#8293=DIRECTION('center_axis',(0.,0.,1.));
#8294=DIRECTION('ref_axis',(1.,0.,0.));
#8295=DIRECTION('axis',(0.,0.,1.));
#8296=DIRECTION('refdir',(1.,0.,0.));
#8297=DIRECTION('center_axis',(0.,0.,1.));
#8298=DIRECTION('ref_axis',(1.,0.,0.));
#8299=DIRECTION('center_axis',(0.,0.,-1.));
#8300=DIRECTION('ref_axis',(1.,0.,0.));
#8301=DIRECTION('',(0.,0.,-1.));
#8302=DIRECTION('center_axis',(0.,0.,-1.));
#8303=DIRECTION('ref_axis',(1.,0.,0.));
#8304=DIRECTION('center_axis',(0.,0.,1.));
#8305=DIRECTION('ref_axis',(1.,0.,0.));
#8306=DIRECTION('center_axis',(0.,0.,1.));
#8307=DIRECTION('ref_axis',(1.,0.,0.));
#8308=DIRECTION('',(0.,0.,-1.));
#8309=DIRECTION('center_axis',(0.,0.,1.));
#8310=DIRECTION('ref_axis',(1.,0.,0.));
#8311=DIRECTION('center_axis',(0.,0.,1.));
#8312=DIRECTION('ref_axis',(1.,0.,0.));
#8313=DIRECTION('center_axis',(0.,0.,1.));
#8314=DIRECTION('ref_axis',(1.,0.,0.));
#8315=DIRECTION('axis',(0.,0.,1.));
#8316=DIRECTION('refdir',(1.,0.,0.));
#8317=DIRECTION('center_axis',(0.,0.,1.));
#8318=DIRECTION('ref_axis',(1.,0.,0.));
#8319=DIRECTION('center_axis',(0.,0.,-1.));
#8320=DIRECTION('ref_axis',(1.,0.,0.));
#8321=DIRECTION('',(0.,0.,-1.));
#8322=DIRECTION('center_axis',(0.,0.,-1.));
#8323=DIRECTION('ref_axis',(1.,0.,0.));
#8324=DIRECTION('center_axis',(0.,0.,1.));
#8325=DIRECTION('ref_axis',(1.,0.,0.));
#8326=DIRECTION('center_axis',(0.,0.,1.));
#8327=DIRECTION('ref_axis',(1.,0.,0.));
#8328=DIRECTION('',(0.,0.,-1.));
#8329=DIRECTION('center_axis',(0.,0.,1.));
#8330=DIRECTION('ref_axis',(1.,0.,0.));
#8331=DIRECTION('center_axis',(0.,0.,1.));
#8332=DIRECTION('ref_axis',(1.,0.,0.));
#8333=DIRECTION('center_axis',(0.,0.,1.));
#8334=DIRECTION('ref_axis',(1.,0.,0.));
#8335=DIRECTION('axis',(0.,0.,1.));
#8336=DIRECTION('refdir',(1.,0.,0.));
#8337=DIRECTION('center_axis',(0.866025403784439,0.,-0.5));
#8338=DIRECTION('ref_axis',(0.5,0.,0.866025403784439));
#8339=DIRECTION('',(-0.5,0.,-0.866025403784439));
#8340=DIRECTION('',(0.,-1.,0.));
#8341=DIRECTION('',(0.5,0.,0.866025403784439));
#8342=DIRECTION('',(0.,-1.,0.));
#8343=DIRECTION('center_axis',(1.60246890531964E-16,0.,-1.));
#8344=DIRECTION('ref_axis',(1.,0.,1.60246890531964E-16));
#8345=DIRECTION('',(-1.,0.,-1.60246890531964E-16));
#8346=DIRECTION('',(0.,-1.,0.));
#8347=DIRECTION('',(1.,0.,1.60246890531964E-16));
#8348=DIRECTION('center_axis',(-0.866025403784439,0.,-0.5));
#8349=DIRECTION('ref_axis',(0.5,0.,-0.866025403784439));
#8350=DIRECTION('',(-0.5,0.,0.866025403784439));
#8351=DIRECTION('',(0.,-1.,0.));
#8352=DIRECTION('',(0.5,0.,-0.866025403784439));
#8353=DIRECTION('center_axis',(-0.866025403784439,0.,0.5));
#8354=DIRECTION('ref_axis',(-0.5,0.,-0.866025403784439));
#8355=DIRECTION('',(0.5,0.,0.866025403784439));
#8356=DIRECTION('',(0.,-1.,0.));
#8357=DIRECTION('',(-0.5,0.,-0.866025403784439));
#8358=DIRECTION('center_axis',(-1.60246890531964E-16,0.,1.));
#8359=DIRECTION('ref_axis',(-1.,0.,-1.60246890531964E-16));
#8360=DIRECTION('',(1.,0.,1.60246890531964E-16));
#8361=DIRECTION('',(0.,-1.,0.));
#8362=DIRECTION('',(-1.,0.,-1.60246890531964E-16));
#8363=DIRECTION('center_axis',(0.866025403784439,0.,0.5));
#8364=DIRECTION('ref_axis',(-0.5,0.,0.866025403784439));
#8365=DIRECTION('',(0.5,0.,-0.866025403784439));
#8366=DIRECTION('',(-0.5,0.,0.866025403784439));
#8367=DIRECTION('center_axis',(0.,1.,0.));
#8368=DIRECTION('ref_axis',(1.,0.,0.));
#8369=DIRECTION('center_axis',(0.,-1.,0.));
#8370=DIRECTION('ref_axis',(0.,0.,-1.));
#8371=DIRECTION('center_axis',(0.,1.,0.));
#8372=DIRECTION('ref_axis',(1.,0.,0.));
#8373=DIRECTION('center_axis',(0.,1.,0.));
#8374=DIRECTION('ref_axis',(1.,0.,0.));
#8375=DIRECTION('center_axis',(0.,1.,0.));
#8376=DIRECTION('ref_axis',(0.,0.,1.));
#8377=DIRECTION('center_axis',(0.,-1.,0.));
#8378=DIRECTION('ref_axis',(1.,0.,0.));
#8379=DIRECTION('center_axis',(0.,-1.,0.));
#8380=DIRECTION('ref_axis',(1.,0.,0.));
#8381=DIRECTION('center_axis',(0.,-1.,0.));
#8382=DIRECTION('ref_axis',(1.,0.,0.));
#8383=DIRECTION('',(0.707106781186547,0.707106781186548,8.65956056235493E-17));
#8384=DIRECTION('center_axis',(0.,-1.,0.));
#8385=DIRECTION('ref_axis',(1.,0.,0.));
#8386=DIRECTION('center_axis',(0.,-1.,0.));
#8387=DIRECTION('ref_axis',(1.,0.,0.));
#8388=DIRECTION('',(0.,1.,0.));
#8389=DIRECTION('center_axis',(0.,1.,0.));
#8390=DIRECTION('ref_axis',(1.,0.,0.));
#8391=DIRECTION('center_axis',(0.,-1.,0.));
#8392=DIRECTION('ref_axis',(1.,0.,0.));
#8393=DIRECTION('',(-0.707106781186547,0.707106781186548,-8.65956056235493E-17));
#8394=DIRECTION('center_axis',(0.,-1.,0.));
#8395=DIRECTION('ref_axis',(0.,0.,-1.));
#8396=DIRECTION('center_axis',(0.,-1.,0.));
#8397=DIRECTION('ref_axis',(1.,0.,0.));
#8398=DIRECTION('center_axis',(0.,1.,0.));
#8399=DIRECTION('ref_axis',(1.,0.,0.));
#8400=DIRECTION('center_axis',(0.,1.,0.));
#8401=DIRECTION('ref_axis',(1.,0.,0.));
#8402=DIRECTION('',(-0.447213595499958,0.894427190999916,-5.47678698264203E-17));
#8403=DIRECTION('center_axis',(0.,-1.,0.));
#8404=DIRECTION('ref_axis',(1.,0.,0.));
#8405=DIRECTION('',(0.,1.,0.));
#8406=DIRECTION('',(0.,0.,1.));
#8407=DIRECTION('',(1.,0.,0.));
#8408=DIRECTION('',(0.,-1.,2.22044604925031E-16));
#8409=DIRECTION('',(1.,0.,0.));
#8410=DIRECTION('',(0.,-1.,2.22044604925031E-16));
#8411=DIRECTION('',(1.,0.,0.));
#8412=DIRECTION('',(0.,-1.,2.22044604925031E-16));
#8413=DIRECTION('',(1.,0.,0.));
#8414=DIRECTION('',(0.,-1.,2.22044604925031E-16));
#8415=DIRECTION('',(1.,0.,0.));
#8416=DIRECTION('',(0.,0.,1.));
#8417=DIRECTION('',(1.,0.,0.));
#8418=DIRECTION('',(0.,0.,1.));
#8419=DIRECTION('',(1.,0.,0.));
#8420=DIRECTION('',(0.,-1.,2.22044604925031E-16));
#8421=DIRECTION('',(1.,0.,0.));
#8422=DIRECTION('',(0.,-1.,2.22044604925031E-16));
#8423=DIRECTION('',(1.,0.,0.));
#8424=DIRECTION('',(0.,-1.,2.22044604925031E-16));
#8425=DIRECTION('',(1.,0.,0.));
#8426=DIRECTION('',(0.,-1.,2.22044604925031E-16));
#8427=DIRECTION('',(1.,0.,0.));
#8428=DIRECTION('',(0.,-1.,2.22044604925031E-16));
#8429=DIRECTION('',(1.,0.,0.));
#8430=DIRECTION('',(0.,0.,1.));
#8431=DIRECTION('',(1.,0.,0.));
#8432=DIRECTION('',(0.,0.,1.));
#8433=DIRECTION('',(1.,0.,0.));
#8434=DIRECTION('',(0.,-1.,2.22044604925031E-16));
#8435=DIRECTION('',(1.,0.,0.));
#8436=DIRECTION('',(0.,-1.,2.22044604925031E-16));
#8437=DIRECTION('',(1.,0.,0.));
#8438=DIRECTION('',(0.,-1.,2.22044604925031E-16));
#8439=DIRECTION('',(1.,0.,0.));
#8440=DIRECTION('',(0.,0.,1.));
#8441=DIRECTION('',(1.,0.,0.));
#8442=DIRECTION('',(0.,-1.,2.22044604925031E-16));
#8443=DIRECTION('',(1.,0.,0.));
#8444=DIRECTION('',(0.,-1.,2.22044604925031E-16));
#8445=DIRECTION('',(1.,0.,0.));
#8446=DIRECTION('',(0.,-1.,2.22044604925031E-16));
#8447=DIRECTION('',(1.,0.,0.));
#8448=DIRECTION('',(0.,0.,1.));
#8449=DIRECTION('',(1.,0.,0.));
#8450=DIRECTION('',(0.,0.,1.));
#8451=DIRECTION('',(1.,0.,0.));
#8452=DIRECTION('',(0.,0.,1.));
#8453=DIRECTION('',(1.,0.,0.));
#8454=DIRECTION('',(0.,0.,1.));
#8455=DIRECTION('',(1.,0.,0.));
#8456=DIRECTION('',(0.,1.,2.22044604925031E-16));
#8457=DIRECTION('',(1.,0.,0.));
#8458=DIRECTION('',(0.,0.,1.));
#8459=DIRECTION('',(2.22044604925031E-16,-1.,0.));
#8460=DIRECTION('',(0.,0.,1.));
#8461=DIRECTION('',(1.,0.,0.));
#8462=DIRECTION('',(0.,0.,1.));
#8463=DIRECTION('',(1.,0.,0.));
#8464=DIRECTION('',(0.,0.,1.));
#8465=DIRECTION('',(1.,0.,0.));
#8466=DIRECTION('',(0.,0.,1.));
#8467=DIRECTION('',(1.,0.,0.));
#8468=DIRECTION('',(0.,-1.,2.22044604925031E-16));
#8469=DIRECTION('',(1.,0.,0.));
#8470=DIRECTION('',(0.,0.,1.));
#8471=DIRECTION('',(1.,0.,0.));
#8472=DIRECTION('',(0.,0.,1.));
#8473=DIRECTION('',(1.,0.,0.));
#8474=DIRECTION('',(0.,0.,1.));
#8475=DIRECTION('',(1.,0.,0.));
#8476=DIRECTION('',(0.,0.,1.));
#8477=DIRECTION('',(2.22044604925031E-16,-1.,0.));
#8478=DIRECTION('',(0.,0.,1.));
#8479=DIRECTION('',(1.,0.,0.));
#8480=DIRECTION('',(0.,0.,1.));
#8481=DIRECTION('',(-1.,1.22464679914735E-16,0.));
#8482=DIRECTION('',(0.,0.,1.));
#8483=DIRECTION('',(2.22044604925031E-16,1.,0.));
#8484=DIRECTION('',(0.,0.,1.));
#8485=DIRECTION('',(2.22044604925031E-16,1.,0.));
#8486=DIRECTION('',(0.,0.,1.));
#8487=DIRECTION('',(2.22044604925031E-16,1.,0.));
#8488=DIRECTION('',(0.,0.,1.));
#8489=DIRECTION('',(2.22044604925031E-16,1.,0.));
#8490=DIRECTION('',(0.,0.,1.));
#8491=DIRECTION('',(2.22044604925031E-16,-1.,0.));
#8492=DIRECTION('',(0.,0.,1.));
#8493=DIRECTION('',(2.22044604925031E-16,-1.,0.));
#8494=DIRECTION('',(0.,0.,1.));
#8495=DIRECTION('',(2.22044604925031E-16,-1.,0.));
#8496=DIRECTION('',(0.,0.,1.));
#8497=DIRECTION('',(2.22044604925031E-16,-1.,0.));
#8498=DIRECTION('',(0.,0.,1.));
#8499=DIRECTION('',(1.,0.,0.));
#8500=DIRECTION('',(0.,0.,1.));
#8501=DIRECTION('',(1.,0.,0.));
#8502=DIRECTION('',(0.,-1.,2.22044604925031E-16));
#8503=DIRECTION('',(1.,0.,0.));
#8504=DIRECTION('',(0.,0.,1.));
#8505=DIRECTION('',(1.,0.,0.));
#8506=DIRECTION('',(6.12259039388532E-17,8.24327257502527E-23,1.));
#8507=DIRECTION('',(0.943995780370468,0.329957522482442,-5.7797022166943E-17));
#8508=DIRECTION('',(-1.37638159375981E-19,7.07996218514644E-20,1.));
#8509=DIRECTION('',(0.999888028329358,0.0149643176800457,1.36563279768267E-19));
#8510=DIRECTION('',(6.12323399573677E-17,0.,1.));
#8511=DIRECTION('',(1.,0.,-6.12323399573677E-17));
#8512=CARTESIAN_POINT('',(0.,0.,0.));
#8513=CARTESIAN_POINT('',(0.,0.,0.));
#8514=CARTESIAN_POINT('',(0.,0.,0.));
#8515=CARTESIAN_POINT('Origin',(11.,2.9,-0.1));
#8516=CARTESIAN_POINT('',(10.835,2.9,0.));
#8517=CARTESIAN_POINT('Origin',(11.,2.9,0.));
#8518=CARTESIAN_POINT('',(10.835,2.9,1.));
#8519=CARTESIAN_POINT('',(10.835,2.9,-0.1));
#8520=CARTESIAN_POINT('Origin',(11.,2.9,1.));
#8521=CARTESIAN_POINT('Origin',(11.,5.1,-0.1));
#8522=CARTESIAN_POINT('',(10.835,5.1,0.));
#8523=CARTESIAN_POINT('Origin',(11.,5.1,0.));
#8524=CARTESIAN_POINT('',(10.835,5.1,1.));
#8525=CARTESIAN_POINT('',(10.835,5.1,-0.1));
#8526=CARTESIAN_POINT('Origin',(11.,5.1,1.));
#8527=CARTESIAN_POINT('Origin',(4.,2.9,-0.1));
#8528=CARTESIAN_POINT('',(3.835,2.9,0.));
#8529=CARTESIAN_POINT('Origin',(4.,2.9,0.));
#8530=CARTESIAN_POINT('',(3.835,2.9,1.));
#8531=CARTESIAN_POINT('',(3.835,2.9,-0.1));
#8532=CARTESIAN_POINT('Origin',(4.,2.9,1.));
#8533=CARTESIAN_POINT('Origin',(4.,5.1,-0.1));
#8534=CARTESIAN_POINT('',(3.835,5.1,0.));
#8535=CARTESIAN_POINT('Origin',(4.,5.1,0.));
#8536=CARTESIAN_POINT('',(3.835,5.1,1.));
#8537=CARTESIAN_POINT('',(3.835,5.1,-0.1));
#8538=CARTESIAN_POINT('Origin',(4.,5.1,1.));
#8539=CARTESIAN_POINT('Origin',(-1.76776695296637,-1.76776695296637,-0.1));
#8540=CARTESIAN_POINT('',(-1.97776695296637,-1.76776695296637,0.));
#8541=CARTESIAN_POINT('Origin',(-1.76776695296637,-1.76776695296637,0.));
#8542=CARTESIAN_POINT('',(-1.97776695296637,-1.76776695296637,1.));
#8543=CARTESIAN_POINT('',(-1.97776695296637,-1.76776695296637,-0.1));
#8544=CARTESIAN_POINT('Origin',(-1.76776695296637,-1.76776695296637,1.));
#8545=CARTESIAN_POINT('Origin',(-1.76776695296637,1.76776695296637,-0.1));
#8546=CARTESIAN_POINT('',(-1.97776695296637,1.76776695296637,0.));
#8547=CARTESIAN_POINT('Origin',(-1.76776695296637,1.76776695296637,0.));
#8548=CARTESIAN_POINT('',(-1.97776695296637,1.76776695296637,1.));
#8549=CARTESIAN_POINT('',(-1.97776695296637,1.76776695296637,-0.1));
#8550=CARTESIAN_POINT('Origin',(-1.76776695296637,1.76776695296637,1.));
#8551=CARTESIAN_POINT('Origin',(1.76776695296637,1.76776695296637,-0.1));
#8552=CARTESIAN_POINT('',(1.55776695296637,1.76776695296637,0.));
#8553=CARTESIAN_POINT('Origin',(1.76776695296637,1.76776695296637,0.));
#8554=CARTESIAN_POINT('',(1.55776695296637,1.76776695296637,1.));
#8555=CARTESIAN_POINT('',(1.55776695296637,1.76776695296637,-0.1));
#8556=CARTESIAN_POINT('Origin',(1.76776695296637,1.76776695296637,1.));
#8557=CARTESIAN_POINT('Origin',(1.76776695296637,-1.76776695296637,-0.1));
#8558=CARTESIAN_POINT('',(1.55776695296637,-1.76776695296637,0.));
#8559=CARTESIAN_POINT('Origin',(1.76776695296637,-1.76776695296637,0.));
#8560=CARTESIAN_POINT('',(1.55776695296637,-1.76776695296637,1.));
#8561=CARTESIAN_POINT('',(1.55776695296637,-1.76776695296637,-0.1));
#8562=CARTESIAN_POINT('Origin',(1.76776695296637,-1.76776695296637,1.));
#8563=CARTESIAN_POINT('Origin',(11.5,6.5,0.));
#8564=CARTESIAN_POINT('',(11.5,6.5,0.));
#8565=CARTESIAN_POINT('',(-3.5,6.5,0.));
#8566=CARTESIAN_POINT('',(11.5,6.5,0.));
#8567=CARTESIAN_POINT('',(-3.5,6.5,1.));
#8568=CARTESIAN_POINT('',(-3.5,6.5,0.));
#8569=CARTESIAN_POINT('',(11.5,6.5,1.));
#8570=CARTESIAN_POINT('',(11.5,6.5,1.));
#8571=CARTESIAN_POINT('',(11.5,6.5,0.));
#8572=CARTESIAN_POINT('Origin',(11.5,-3.5,0.));
#8573=CARTESIAN_POINT('',(11.5,-3.5,0.));
#8574=CARTESIAN_POINT('',(11.5,-3.5,0.));
#8575=CARTESIAN_POINT('',(11.5,-3.5,1.));
#8576=CARTESIAN_POINT('',(11.5,-3.5,1.));
#8577=CARTESIAN_POINT('',(11.5,-3.5,0.));
#8578=CARTESIAN_POINT('Origin',(-3.5,-3.5,0.));
#8579=CARTESIAN_POINT('',(-3.5,-3.5,0.));
#8580=CARTESIAN_POINT('',(-3.5,-3.5,0.));
#8581=CARTESIAN_POINT('',(-3.5,-3.5,1.));
#8582=CARTESIAN_POINT('',(-3.5,-3.5,1.));
#8583=CARTESIAN_POINT('',(-3.5,-3.5,0.));
#8584=CARTESIAN_POINT('Origin',(-3.5,6.5,0.));
#8585=CARTESIAN_POINT('',(-3.5,6.5,0.));
#8586=CARTESIAN_POINT('',(-3.5,6.5,1.));
#8587=CARTESIAN_POINT('Origin',(4.,1.5,1.));
#8588=CARTESIAN_POINT('Origin',(4.,1.5,0.));
#8589=CARTESIAN_POINT('',(0.,0.,0.));
#8590=CARTESIAN_POINT('Origin',(0.115470053837925,-0.5,-0.2));
#8591=CARTESIAN_POINT('',(0.23094010767585,-0.5,0.));
#8592=CARTESIAN_POINT('',(0.115470053837925,-0.5,-0.2));
#8593=CARTESIAN_POINT('',(0.23094010767585,-0.5,0.));
#8594=CARTESIAN_POINT('',(0.115470053837925,-0.8,-0.2));
#8595=CARTESIAN_POINT('',(0.115470053837925,-0.5,-0.2));
#8596=CARTESIAN_POINT('',(0.23094010767585,-0.8,0.));
#8597=CARTESIAN_POINT('',(0.23094010767585,-0.8,0.));
#8598=CARTESIAN_POINT('',(0.23094010767585,-0.5,0.));
#8599=CARTESIAN_POINT('Origin',(-0.115470053837925,-0.5,-0.2));
#8600=CARTESIAN_POINT('',(-0.115470053837925,-0.5,-0.2));
#8601=CARTESIAN_POINT('',(0.115470053837925,-0.5,-0.2));
#8602=CARTESIAN_POINT('',(-0.115470053837925,-0.8,-0.2));
#8603=CARTESIAN_POINT('',(-0.115470053837925,-0.5,-0.2));
#8604=CARTESIAN_POINT('',(0.115470053837925,-0.8,-0.2));
#8605=CARTESIAN_POINT('Origin',(-0.23094010767585,-0.5,-2.77555756156289E-17));
#8606=CARTESIAN_POINT('',(-0.23094010767585,-0.5,-2.82820063659975E-17));
#8607=CARTESIAN_POINT('',(-0.115470053837925,-0.5,-0.2));
#8608=CARTESIAN_POINT('',(-0.23094010767585,-0.8,-2.77555756156289E-17));
#8609=CARTESIAN_POINT('',(-0.23094010767585,-0.5,-2.82820063659975E-17));
#8610=CARTESIAN_POINT('',(-0.115470053837925,-0.8,-0.2));
#8611=CARTESIAN_POINT('Origin',(-0.115470053837925,-0.5,0.2));
#8612=CARTESIAN_POINT('',(-0.115470053837925,-0.5,0.2));
#8613=CARTESIAN_POINT('',(-0.23094010767585,-0.5,-2.82820063659975E-17));
#8614=CARTESIAN_POINT('',(-0.115470053837925,-0.8,0.2));
#8615=CARTESIAN_POINT('',(-0.115470053837925,-0.5,0.2));
#8616=CARTESIAN_POINT('',(-0.23094010767585,-0.8,-2.82820063659975E-17));
#8617=CARTESIAN_POINT('Origin',(0.115470053837925,-0.5,0.2));
#8618=CARTESIAN_POINT('',(0.115470053837925,-0.5,0.2));
#8619=CARTESIAN_POINT('',(-0.115470053837925,-0.5,0.2));
#8620=CARTESIAN_POINT('',(0.115470053837925,-0.8,0.2));
#8621=CARTESIAN_POINT('',(0.115470053837925,-0.5,0.2));
#8622=CARTESIAN_POINT('',(-0.115470053837925,-0.8,0.2));
#8623=CARTESIAN_POINT('Origin',(0.23094010767585,-0.5,0.));
#8624=CARTESIAN_POINT('',(0.115470053837925,-0.5,0.2));
#8625=CARTESIAN_POINT('',(0.115470053837925,-0.8,0.2));
#8626=CARTESIAN_POINT('Origin',(0.,-0.5,0.));
#8627=CARTESIAN_POINT('Origin',(0.,-0.8,0.));
#8628=CARTESIAN_POINT('Origin',(0.,-1.4,0.));
#8629=CARTESIAN_POINT('',(-0.24505,-1.4,3.00099698131059E-17));
#8630=CARTESIAN_POINT('Origin',(0.,-1.4,0.));
#8631=CARTESIAN_POINT('Origin',(0.375,0.5,0.));
#8632=CARTESIAN_POINT('',(-0.375,0.5,-4.59242549680257E-17));
#8633=CARTESIAN_POINT('Origin',(0.,0.5,0.));
#8634=CARTESIAN_POINT('Origin',(0.,0.475,0.));
#8635=CARTESIAN_POINT('',(-0.425,0.45,-5.20474889637625E-17));
#8636=CARTESIAN_POINT('Origin',(0.,0.45,0.));
#8637=CARTESIAN_POINT('',(-0.4,0.475,-4.89858719658941E-17));
#8638=CARTESIAN_POINT('Origin',(0.,0.24,0.));
#8639=CARTESIAN_POINT('',(-0.425,0.0299999999999998,-5.20474889637625E-17));
#8640=CARTESIAN_POINT('Origin',(0.,0.0299999999999998,0.));
#8641=CARTESIAN_POINT('',(-0.425,0.24,-5.20474889637625E-17));
#8642=CARTESIAN_POINT('Origin',(0.,0.0150000000000001,0.));
#8643=CARTESIAN_POINT('',(-0.395,4.85722573273506E-17,-4.83735485663204E-17));
#8644=CARTESIAN_POINT('Origin',(0.,0.,0.));
#8645=CARTESIAN_POINT('',(-0.41,0.0150000000000001,-5.02105187650415E-17));
#8646=CARTESIAN_POINT('Origin',(0.27,0.,0.));
#8647=CARTESIAN_POINT('',(-0.27,0.,-3.30654635769785E-17));
#8648=CARTESIAN_POINT('Origin',(0.,0.,0.));
#8649=CARTESIAN_POINT('Origin',(0.,-0.02,0.));
#8650=CARTESIAN_POINT('',(-0.24505,-0.0498999999999999,3.00099698131059E-17));
#8651=CARTESIAN_POINT('Origin',(0.,-0.0498999999999999,0.));
#8652=CARTESIAN_POINT('',(-0.26,-0.02,-3.18408167778312E-17));
#8653=CARTESIAN_POINT('Origin',(0.,-0.995,0.));
#8654=CARTESIAN_POINT('',(-0.24505,-0.995,-3.00099698131059E-17));
#8655=CARTESIAN_POINT('',(0.,0.,0.));
#8656=CARTESIAN_POINT('Origin',(0.9,0.,1.4));
#8657=CARTESIAN_POINT('',(0.988888264668966,0.25,1.4));
#8658=CARTESIAN_POINT('',(1.02,-1.18386380373883E-17,1.65));
#8659=CARTESIAN_POINT('Ctrl Pts',(0.988888264668966,0.25,1.4));
#8660=CARTESIAN_POINT('Ctrl Pts',(0.988888264668966,0.25,1.43153139415882));
#8661=CARTESIAN_POINT('Ctrl Pts',(0.990553370646674,0.243672048431404,1.46507214966317));
#8662=CARTESIAN_POINT('Ctrl Pts',(0.996491737296663,0.218119830014375,1.52662620974954));
#8663=CARTESIAN_POINT('Ctrl Pts',(1.00067109353237,0.198902128206072,1.5546512623872));
#8664=CARTESIAN_POINT('Ctrl Pts',(1.00845756932386,0.154654113568716,1.59889927702456));
#8665=CARTESIAN_POINT('Ctrl Pts',(1.01258144235289,0.126627870945253,1.61811920309393));
#8666=CARTESIAN_POINT('Ctrl Pts',(1.0183917429657,0.065069600391363,1.64367304400768));
#8667=CARTESIAN_POINT('Ctrl Pts',(1.02,0.031527330883376,1.65));
#8668=CARTESIAN_POINT('Ctrl Pts',(1.02,2.77555756156289E-17,1.65));
#8669=CARTESIAN_POINT('Ctrl Pts',(1.02,6.93889390390723E-18,1.65));
#8670=CARTESIAN_POINT('Ctrl Pts',(1.02,-0.031527330883376,1.65));
#8671=CARTESIAN_POINT('Ctrl Pts',(1.0183917429657,-0.065069600391363,1.64367304400768));
#8672=CARTESIAN_POINT('Ctrl Pts',(1.01258144235289,-0.126627870945253,1.61811920309393));
#8673=CARTESIAN_POINT('Ctrl Pts',(1.00845756932386,-0.154654113568716,1.59889927702456));
#8674=CARTESIAN_POINT('Ctrl Pts',(1.00067109353237,-0.198902128206072,1.5546512623872));
#8675=CARTESIAN_POINT('Ctrl Pts',(0.996491737296663,-0.218119830014375,
1.52662620974954));
#8676=CARTESIAN_POINT('Ctrl Pts',(0.990553370646674,-0.243672048431404,
1.46507214966317));
#8677=CARTESIAN_POINT('Ctrl Pts',(0.988888264668967,-0.25,1.43153139415882));
#8678=CARTESIAN_POINT('Ctrl Pts',(0.988888264668967,-0.25,1.36846860584118));
#8679=CARTESIAN_POINT('Ctrl Pts',(0.990553370646674,-0.243672048431404,
1.33492785033683));
#8680=CARTESIAN_POINT('Ctrl Pts',(0.996491737296663,-0.218119830014375,
1.27337379025046));
#8681=CARTESIAN_POINT('Ctrl Pts',(1.00067109353237,-0.198902128206072,1.2453487376128));
#8682=CARTESIAN_POINT('Ctrl Pts',(1.00845756932386,-0.154654113568716,1.20110072297544));
#8683=CARTESIAN_POINT('Ctrl Pts',(1.01258144235289,-0.126627870945254,1.18188079690607));
#8684=CARTESIAN_POINT('Ctrl Pts',(1.0183917429657,-0.0650696003913633,1.15632695599232));
#8685=CARTESIAN_POINT('Ctrl Pts',(1.02,-0.0315273308833761,1.15));
#8686=CARTESIAN_POINT('Ctrl Pts',(1.02,0.0315273308833759,1.15));
#8687=CARTESIAN_POINT('Ctrl Pts',(1.0183917429657,0.065069600391363,1.15632695599232));
#8688=CARTESIAN_POINT('Ctrl Pts',(1.01258144235289,0.126627870945253,1.18188079690607));
#8689=CARTESIAN_POINT('Ctrl Pts',(1.00845756932386,0.154654113568716,1.20110072297544));
#8690=CARTESIAN_POINT('Ctrl Pts',(1.00067109353237,0.198902128206072,1.2453487376128));
#8691=CARTESIAN_POINT('Ctrl Pts',(0.996491737296663,0.218119830014375,1.27337379025046));
#8692=CARTESIAN_POINT('Ctrl Pts',(0.990553370646674,0.243672048431404,1.33492785033683));
#8693=CARTESIAN_POINT('Ctrl Pts',(0.988888264668967,0.25,1.36846860584118));
#8694=CARTESIAN_POINT('Ctrl Pts',(0.988888264668967,0.25,1.4));
#8695=CARTESIAN_POINT('',(3.,-3.06161699786838E-17,1.65));
#8696=CARTESIAN_POINT('',(0.9,-3.06161699786838E-17,1.65));
#8697=CARTESIAN_POINT('',(2.98956518577535,0.25,1.4));
#8698=CARTESIAN_POINT('Ctrl Pts',(2.98956518577535,0.25,1.4));
#8699=CARTESIAN_POINT('Ctrl Pts',(2.98956518577535,0.25,1.36859378633186));
#8700=CARTESIAN_POINT('Ctrl Pts',(2.99011104995181,0.24372047740942,1.33510417960069));
#8701=CARTESIAN_POINT('Ctrl Pts',(2.99208145165098,0.218202539734559,1.27351367328886));
#8702=CARTESIAN_POINT('Ctrl Pts',(2.99347740802958,0.198964922639276,1.245411532046));
#8703=CARTESIAN_POINT('Ctrl Pts',(2.99609686518216,0.154588504271054,1.20103511367778));
#8704=CARTESIAN_POINT('Ctrl Pts',(2.99749070376198,0.126486346986081,1.18179746841036));
#8705=CARTESIAN_POINT('Ctrl Pts',(2.99945625936844,0.0648957875009219,1.15627950921557));
#8706=CARTESIAN_POINT('Ctrl Pts',(3.,0.0314061622633416,1.15));
#8707=CARTESIAN_POINT('Ctrl Pts',(3.,-0.0314061622633416,1.15));
#8708=CARTESIAN_POINT('Ctrl Pts',(2.99945625936844,-0.0648957875009221,
1.15627950921557));
#8709=CARTESIAN_POINT('Ctrl Pts',(2.99749070376198,-0.126486346986081,1.18179746841036));
#8710=CARTESIAN_POINT('Ctrl Pts',(2.99609686518216,-0.154588504271054,1.20103511367778));
#8711=CARTESIAN_POINT('Ctrl Pts',(2.99347740802958,-0.198964922639276,1.245411532046));
#8712=CARTESIAN_POINT('Ctrl Pts',(2.99208145165098,-0.218202539734559,1.27351367328886));
#8713=CARTESIAN_POINT('Ctrl Pts',(2.99011104995181,-0.24372047740942,1.33510417960069));
#8714=CARTESIAN_POINT('Ctrl Pts',(2.98956518577535,-0.25,1.36859378633186));
#8715=CARTESIAN_POINT('Ctrl Pts',(2.98956518577535,-0.25,1.43140621366814));
#8716=CARTESIAN_POINT('Ctrl Pts',(2.99011104995181,-0.24372047740942,1.4648958203993));
#8717=CARTESIAN_POINT('Ctrl Pts',(2.99208145165098,-0.21820253973456,1.52648632671114));
#8718=CARTESIAN_POINT('Ctrl Pts',(2.99347740802958,-0.198964922639276,1.554588467954));
#8719=CARTESIAN_POINT('Ctrl Pts',(2.99609686518216,-0.154588504271054,1.59896488632222));
#8720=CARTESIAN_POINT('Ctrl Pts',(2.99749070376198,-0.126486346986082,1.61820253158964));
#8721=CARTESIAN_POINT('Ctrl Pts',(2.99945625936844,-0.0648957875009221,
1.64372049078443));
#8722=CARTESIAN_POINT('Ctrl Pts',(3.,-0.0314061622633417,1.65));
#8723=CARTESIAN_POINT('Ctrl Pts',(3.,-5.55111512312578E-17,1.65));
#8724=CARTESIAN_POINT('Ctrl Pts',(3.,-2.08166817117217E-17,1.65));
#8725=CARTESIAN_POINT('Ctrl Pts',(3.,0.0314061622633416,1.65));
#8726=CARTESIAN_POINT('Ctrl Pts',(2.99945625936844,0.0648957875009221,1.64372049078443));
#8727=CARTESIAN_POINT('Ctrl Pts',(2.99749070376198,0.126486346986081,1.61820253158964));
#8728=CARTESIAN_POINT('Ctrl Pts',(2.99609686518216,0.154588504271054,1.59896488632222));
#8729=CARTESIAN_POINT('Ctrl Pts',(2.99347740802958,0.198964922639276,1.554588467954));
#8730=CARTESIAN_POINT('Ctrl Pts',(2.99208145165098,0.218202539734559,1.52648632671114));
#8731=CARTESIAN_POINT('Ctrl Pts',(2.99011104995181,0.24372047740942,1.46489582039931));
#8732=CARTESIAN_POINT('Ctrl Pts',(2.98956518577535,0.25,1.43140621366814));
#8733=CARTESIAN_POINT('Ctrl Pts',(2.98956518577535,0.25,1.4));
#8734=CARTESIAN_POINT('Origin',(-1.23743686707646,-1.23743686707646,2.9));
#8735=CARTESIAN_POINT('',(-1.40243686707646,-1.23743686707646,2.9));
#8736=CARTESIAN_POINT('Origin',(-1.23743686707646,-1.23743686707646,2.9));
#8737=CARTESIAN_POINT('',(-1.40243686707646,-1.23743686707646,3.6));
#8738=CARTESIAN_POINT('',(-1.40243686707646,-1.23743686707646,2.9));
#8739=CARTESIAN_POINT('Origin',(-1.23743686707646,-1.23743686707646,3.6));
#8740=CARTESIAN_POINT('Origin',(-1.23743686707646,-1.23743686707646,2.9));
#8741=CARTESIAN_POINT('Origin',(-1.23743686707646,1.23743686707646,2.9));
#8742=CARTESIAN_POINT('',(-1.40243686707646,1.23743686707646,2.9));
#8743=CARTESIAN_POINT('Origin',(-1.23743686707646,1.23743686707646,2.9));
#8744=CARTESIAN_POINT('',(-1.40243686707646,1.23743686707646,3.6));
#8745=CARTESIAN_POINT('',(-1.40243686707646,1.23743686707646,2.9));
#8746=CARTESIAN_POINT('Origin',(-1.23743686707646,1.23743686707646,3.6));
#8747=CARTESIAN_POINT('Origin',(-1.23743686707646,1.23743686707646,2.9));
#8748=CARTESIAN_POINT('Origin',(1.23743686707646,1.23743686707646,2.9));
#8749=CARTESIAN_POINT('',(1.07243686707646,1.23743686707646,2.9));
#8750=CARTESIAN_POINT('Origin',(1.23743686707646,1.23743686707646,2.9));
#8751=CARTESIAN_POINT('',(1.07243686707646,1.23743686707646,3.6));
#8752=CARTESIAN_POINT('',(1.07243686707646,1.23743686707646,2.9));
#8753=CARTESIAN_POINT('Origin',(1.23743686707646,1.23743686707646,3.6));
#8754=CARTESIAN_POINT('Origin',(1.23743686707646,1.23743686707646,2.9));
#8755=CARTESIAN_POINT('Origin',(1.23743686707646,-1.23743686707646,2.9));
#8756=CARTESIAN_POINT('',(1.07243686707646,-1.23743686707646,2.9));
#8757=CARTESIAN_POINT('Origin',(1.23743686707646,-1.23743686707646,2.9));
#8758=CARTESIAN_POINT('',(1.07243686707646,-1.23743686707646,3.6));
#8759=CARTESIAN_POINT('',(1.07243686707646,-1.23743686707646,2.9));
#8760=CARTESIAN_POINT('Origin',(1.23743686707646,-1.23743686707646,3.6));
#8761=CARTESIAN_POINT('Origin',(1.23743686707646,-1.23743686707646,2.9));
#8762=CARTESIAN_POINT('Origin',(-1.76776695296637,-1.76776695296637,2.4));
#8763=CARTESIAN_POINT('',(-1.8139637388702,-1.24480341984751,2.4));
#8764=CARTESIAN_POINT('',(-1.24480341984751,-1.81396373887019,2.4));
#8765=CARTESIAN_POINT('Origin',(0.,0.,2.4));
#8766=CARTESIAN_POINT('Origin',(-1.76776695296637,-1.76776695296637,2.4));
#8767=CARTESIAN_POINT('Origin',(-1.76776695296637,-1.76776695296637,1.8));
#8768=CARTESIAN_POINT('',(-1.8139637388702,-1.24480341984751,1.8));
#8769=CARTESIAN_POINT('',(-1.8139637388702,-1.24480341984751,1.8));
#8770=CARTESIAN_POINT('',(-1.24480341984751,-1.81396373887019,1.8));
#8771=CARTESIAN_POINT('Origin',(-1.76776695296637,-1.76776695296637,1.8));
#8772=CARTESIAN_POINT('',(-1.24480341984751,-1.81396373887019,1.8));
#8773=CARTESIAN_POINT('Origin',(-1.76776695296637,1.76776695296637,1.8));
#8774=CARTESIAN_POINT('',(-1.81396373887019,1.24480341984751,2.4));
#8775=CARTESIAN_POINT('',(-1.81396373887019,1.24480341984751,1.8));
#8776=CARTESIAN_POINT('',(-1.81396373887019,1.24480341984751,1.8));
#8777=CARTESIAN_POINT('',(-1.24480341984751,1.81396373887019,2.4));
#8778=CARTESIAN_POINT('Origin',(-1.76776695296637,1.76776695296637,2.4));
#8779=CARTESIAN_POINT('',(-1.24480341984751,1.81396373887019,1.8));
#8780=CARTESIAN_POINT('',(-1.24480341984751,1.81396373887019,1.8));
#8781=CARTESIAN_POINT('Origin',(-1.76776695296637,1.76776695296637,1.8));
#8782=CARTESIAN_POINT('Origin',(-1.76776695296637,1.76776695296637,2.4));
#8783=CARTESIAN_POINT('Origin',(0.,0.,2.4));
#8784=CARTESIAN_POINT('Origin',(1.76776695296637,1.76776695296637,1.8));
#8785=CARTESIAN_POINT('',(1.24480341984751,1.81396373887019,2.4));
#8786=CARTESIAN_POINT('',(1.24480341984751,1.81396373887019,1.8));
#8787=CARTESIAN_POINT('',(1.24480341984751,1.81396373887019,1.8));
#8788=CARTESIAN_POINT('',(1.81396373887019,1.24480341984751,2.4));
#8789=CARTESIAN_POINT('Origin',(1.76776695296637,1.76776695296637,2.4));
#8790=CARTESIAN_POINT('',(1.81396373887019,1.24480341984751,1.8));
#8791=CARTESIAN_POINT('',(1.81396373887019,1.24480341984751,1.8));
#8792=CARTESIAN_POINT('Origin',(1.76776695296637,1.76776695296637,1.8));
#8793=CARTESIAN_POINT('Origin',(1.76776695296637,1.76776695296637,2.4));
#8794=CARTESIAN_POINT('Origin',(0.,0.,2.4));
#8795=CARTESIAN_POINT('Origin',(1.76776695296637,-1.76776695296637,1.8));
#8796=CARTESIAN_POINT('',(1.81396373887019,-1.24480341984751,2.4));
#8797=CARTESIAN_POINT('',(1.81396373887019,-1.24480341984751,1.8));
#8798=CARTESIAN_POINT('',(1.81396373887019,-1.24480341984751,1.8));
#8799=CARTESIAN_POINT('',(1.24480341984751,-1.8139637388702,2.4));
#8800=CARTESIAN_POINT('Origin',(1.76776695296637,-1.76776695296637,2.4));
#8801=CARTESIAN_POINT('',(1.24480341984751,-1.8139637388702,1.8));
#8802=CARTESIAN_POINT('',(1.24480341984751,-1.8139637388702,1.8));
#8803=CARTESIAN_POINT('Origin',(1.76776695296637,-1.76776695296637,1.8));
#8804=CARTESIAN_POINT('Origin',(1.76776695296637,-1.76776695296637,2.4));
#8805=CARTESIAN_POINT('Origin',(0.,0.,2.4));
#8806=CARTESIAN_POINT('Origin',(0.,0.,1.));
#8807=CARTESIAN_POINT('',(-2.2,-2.69422295812418E-16,3.6));
#8808=CARTESIAN_POINT('Origin',(0.,0.,3.6));
#8809=CARTESIAN_POINT('',(-2.2,-2.69422295812418E-16,1.8));
#8810=CARTESIAN_POINT('',(-2.2,-2.69422295812418E-16,1.));
#8811=CARTESIAN_POINT('Origin',(0.,0.,1.8));
#8812=CARTESIAN_POINT('Origin',(0.,0.,1.8));
#8813=CARTESIAN_POINT('Origin',(0.,0.,1.8));
#8814=CARTESIAN_POINT('Origin',(0.,0.,1.8));
#8815=CARTESIAN_POINT('Origin',(0.,0.,1.8));
#8816=CARTESIAN_POINT('Origin',(0.,0.,1.8));
#8817=CARTESIAN_POINT('',(-3.,-3.67394039744206E-16,1.8));
#8818=CARTESIAN_POINT('Origin',(0.,0.,1.8));
#8819=CARTESIAN_POINT('',(-2.04276695296637,-1.76776695296637,1.8));
#8820=CARTESIAN_POINT('Origin',(-1.76776695296637,-1.76776695296637,1.8));
#8821=CARTESIAN_POINT('',(1.49276695296637,1.76776695296637,1.8));
#8822=CARTESIAN_POINT('Origin',(1.76776695296637,1.76776695296637,1.8));
#8823=CARTESIAN_POINT('',(1.49276695296637,-1.76776695296637,1.8));
#8824=CARTESIAN_POINT('Origin',(1.76776695296637,-1.76776695296637,1.8));
#8825=CARTESIAN_POINT('',(-2.04276695296637,1.76776695296637,1.8));
#8826=CARTESIAN_POINT('Origin',(-1.76776695296637,1.76776695296637,1.8));
#8827=CARTESIAN_POINT('Origin',(-1.76776695296637,-1.76776695296637,0.9));
#8828=CARTESIAN_POINT('',(-2.04276695296637,-1.76776695296637,1.));
#8829=CARTESIAN_POINT('Origin',(-1.76776695296637,-1.76776695296637,1.));
#8830=CARTESIAN_POINT('',(-2.04276695296637,-1.76776695296637,0.9));
#8831=CARTESIAN_POINT('Origin',(-1.76776695296637,1.76776695296637,0.9));
#8832=CARTESIAN_POINT('',(-2.04276695296637,1.76776695296637,1.));
#8833=CARTESIAN_POINT('Origin',(-1.76776695296637,1.76776695296637,1.));
#8834=CARTESIAN_POINT('',(-2.04276695296637,1.76776695296637,0.9));
#8835=CARTESIAN_POINT('Origin',(1.76776695296637,1.76776695296637,0.9));
#8836=CARTESIAN_POINT('',(1.49276695296637,1.76776695296637,1.));
#8837=CARTESIAN_POINT('Origin',(1.76776695296637,1.76776695296637,1.));
#8838=CARTESIAN_POINT('',(1.49276695296637,1.76776695296637,0.9));
#8839=CARTESIAN_POINT('Origin',(1.76776695296637,-1.76776695296637,0.9));
#8840=CARTESIAN_POINT('',(1.49276695296637,-1.76776695296637,1.));
#8841=CARTESIAN_POINT('Origin',(1.76776695296637,-1.76776695296637,1.));
#8842=CARTESIAN_POINT('',(1.49276695296637,-1.76776695296637,0.9));
#8843=CARTESIAN_POINT('Origin',(0.,0.,2.05));
#8844=CARTESIAN_POINT('',(-1.5,-1.83697019872103E-16,2.05));
#8845=CARTESIAN_POINT('Origin',(0.,0.,2.05));
#8846=CARTESIAN_POINT('',(-1.5,1.83697019872103E-16,3.6));
#8847=CARTESIAN_POINT('',(-1.5,-1.83697019872103E-16,2.05));
#8848=CARTESIAN_POINT('Origin',(0.,0.,3.6));
#8849=CARTESIAN_POINT('Origin',(0.,0.,2.05));
#8850=CARTESIAN_POINT('',(-1.02,-1.2491397351303E-16,2.05));
#8851=CARTESIAN_POINT('Origin',(0.,0.,2.05));
#8852=CARTESIAN_POINT('Origin',(0.,0.,1.));
#8853=CARTESIAN_POINT('',(-3.,-3.67394039744206E-16,1.));
#8854=CARTESIAN_POINT('',(-3.,-3.67394039744206E-16,1.));
#8855=CARTESIAN_POINT('Origin',(0.,0.,1.));
#8856=CARTESIAN_POINT('Origin',(0.,0.,1.));
#8857=CARTESIAN_POINT('',(-1.02,-1.2491397351303E-16,1.));
#8858=CARTESIAN_POINT('',(-1.02,-1.2491397351303E-16,1.));
#8859=CARTESIAN_POINT('Origin',(0.,0.,1.));
#8860=CARTESIAN_POINT('Origin',(0.,0.,3.6));
#8861=CARTESIAN_POINT('Origin',(0.,0.,1.));
#8862=CARTESIAN_POINT('',(0.,0.,0.));
#8863=CARTESIAN_POINT('Origin',(-1.23743686707646,-1.23743686707646,4.));
#8864=CARTESIAN_POINT('',(-1.61243686707646,-1.23743686707646,4.));
#8865=CARTESIAN_POINT('Origin',(-1.23743686707646,-1.23743686707646,4.));
#8866=CARTESIAN_POINT('',(-1.61243686707646,-1.23743686707646,4.4));
#8867=CARTESIAN_POINT('',(-1.61243686707646,-1.23743686707646,4.));
#8868=CARTESIAN_POINT('Origin',(-1.23743686707646,-1.23743686707646,4.4));
#8869=CARTESIAN_POINT('Origin',(-1.23743686707646,-1.23743686707646,4.));
#8870=CARTESIAN_POINT('',(-1.46243686707646,-1.23743686707646,4.));
#8871=CARTESIAN_POINT('Origin',(-1.23743686707646,-1.23743686707646,4.));
#8872=CARTESIAN_POINT('Origin',(-1.23743686707646,1.23743686707646,4.));
#8873=CARTESIAN_POINT('',(-1.61243686707646,1.23743686707646,4.));
#8874=CARTESIAN_POINT('Origin',(-1.23743686707646,1.23743686707646,4.));
#8875=CARTESIAN_POINT('',(-1.61243686707646,1.23743686707646,4.4));
#8876=CARTESIAN_POINT('',(-1.61243686707646,1.23743686707646,4.));
#8877=CARTESIAN_POINT('Origin',(-1.23743686707646,1.23743686707646,4.4));
#8878=CARTESIAN_POINT('Origin',(-1.23743686707646,1.23743686707646,4.));
#8879=CARTESIAN_POINT('',(-1.46243686707646,1.23743686707646,4.));
#8880=CARTESIAN_POINT('Origin',(-1.23743686707646,1.23743686707646,4.));
#8881=CARTESIAN_POINT('Origin',(1.23743686707646,1.23743686707646,4.));
#8882=CARTESIAN_POINT('',(0.862436867076458,1.23743686707646,4.));
#8883=CARTESIAN_POINT('Origin',(1.23743686707646,1.23743686707646,4.));
#8884=CARTESIAN_POINT('',(0.862436867076458,1.23743686707646,4.4));
#8885=CARTESIAN_POINT('',(0.862436867076458,1.23743686707646,4.));
#8886=CARTESIAN_POINT('Origin',(1.23743686707646,1.23743686707646,4.4));
#8887=CARTESIAN_POINT('Origin',(1.23743686707646,1.23743686707646,4.));
#8888=CARTESIAN_POINT('',(1.01243686707646,1.23743686707646,4.));
#8889=CARTESIAN_POINT('Origin',(1.23743686707646,1.23743686707646,4.));
#8890=CARTESIAN_POINT('Origin',(1.23743686707646,-1.23743686707646,4.));
#8891=CARTESIAN_POINT('',(0.862436867076458,-1.23743686707646,4.));
#8892=CARTESIAN_POINT('Origin',(1.23743686707646,-1.23743686707646,4.));
#8893=CARTESIAN_POINT('',(0.862436867076458,-1.23743686707646,4.4));
#8894=CARTESIAN_POINT('',(0.862436867076458,-1.23743686707646,4.));
#8895=CARTESIAN_POINT('Origin',(1.23743686707646,-1.23743686707646,4.4));
#8896=CARTESIAN_POINT('Origin',(1.23743686707646,-1.23743686707646,4.));
#8897=CARTESIAN_POINT('',(1.01243686707646,-1.23743686707646,4.));
#8898=CARTESIAN_POINT('Origin',(1.23743686707646,-1.23743686707646,4.));
#8899=CARTESIAN_POINT('Origin',(-1.23743686707646,-1.23743686707646,3.5));
#8900=CARTESIAN_POINT('',(-1.46243686707646,-1.23743686707646,3.6));
#8901=CARTESIAN_POINT('Origin',(-1.23743686707646,-1.23743686707646,3.6));
#8902=CARTESIAN_POINT('',(-1.46243686707646,-1.23743686707646,3.5));
#8903=CARTESIAN_POINT('Origin',(-1.23743686707646,1.23743686707646,3.5));
#8904=CARTESIAN_POINT('',(-1.46243686707646,1.23743686707646,3.6));
#8905=CARTESIAN_POINT('Origin',(-1.23743686707646,1.23743686707646,3.6));
#8906=CARTESIAN_POINT('',(-1.46243686707646,1.23743686707646,3.5));
#8907=CARTESIAN_POINT('Origin',(1.23743686707646,1.23743686707646,3.5));
#8908=CARTESIAN_POINT('',(1.01243686707646,1.23743686707646,3.6));
#8909=CARTESIAN_POINT('Origin',(1.23743686707646,1.23743686707646,3.6));
#8910=CARTESIAN_POINT('',(1.01243686707646,1.23743686707646,3.5));
#8911=CARTESIAN_POINT('Origin',(1.23743686707646,-1.23743686707646,3.5));
#8912=CARTESIAN_POINT('',(1.01243686707646,-1.23743686707646,3.6));
#8913=CARTESIAN_POINT('Origin',(1.23743686707646,-1.23743686707646,3.6));
#8914=CARTESIAN_POINT('',(1.01243686707646,-1.23743686707646,3.5));
#8915=CARTESIAN_POINT('Origin',(0.,0.,2.95));
#8916=CARTESIAN_POINT('',(-1.49,-1.82472373072956E-16,3.6));
#8917=CARTESIAN_POINT('Origin',(0.,0.,3.6));
#8918=CARTESIAN_POINT('',(-1.49,-1.82472373072956E-16,2.95));
#8919=CARTESIAN_POINT('',(-1.49,-1.82472373072956E-16,2.95));
#8920=CARTESIAN_POINT('Origin',(0.,0.,2.95));
#8921=CARTESIAN_POINT('Origin',(0.,0.,2.95));
#8922=CARTESIAN_POINT('',(-0.71,-8.69499227394621E-17,2.95));
#8923=CARTESIAN_POINT('Origin',(0.,0.,2.95));
#8924=CARTESIAN_POINT('Origin',(0.,0.,3.6));
#8925=CARTESIAN_POINT('',(-0.71,-8.69499227394621E-17,4.4));
#8926=CARTESIAN_POINT('Origin',(0.,0.,4.4));
#8927=CARTESIAN_POINT('',(-0.71,-8.69499227394621E-17,3.6));
#8928=CARTESIAN_POINT('Origin',(0.,0.,3.6));
#8929=CARTESIAN_POINT('',(-2.2,-2.69422295812418E-16,4.4));
#8930=CARTESIAN_POINT('Origin',(0.,0.,4.4));
#8931=CARTESIAN_POINT('',(-2.2,-2.69422295812418E-16,3.6));
#8932=CARTESIAN_POINT('',(-2.2,-2.69422295812418E-16,3.6));
#8933=CARTESIAN_POINT('Origin',(0.,0.,3.6));
#8934=CARTESIAN_POINT('Origin',(0.,0.,4.4));
#8935=CARTESIAN_POINT('Origin',(0.,0.,3.6));
#8936=CARTESIAN_POINT('',(0.,0.,0.));
#8937=CARTESIAN_POINT('',(0.,0.,0.));
#8938=CARTESIAN_POINT('Origin',(0.,0.,0.));
#8939=CARTESIAN_POINT('',(-0.976185,-0.246528389340863,-1.19548183562566E-16));
#8940=CARTESIAN_POINT('',(-1.19548183562566E-16,-0.246528389340863,0.976185));
#8941=CARTESIAN_POINT('Origin',(0.,-0.246528389340863,0.));
#8942=CARTESIAN_POINT('Origin',(0.,-0.246528389340863,0.));
#8943=CARTESIAN_POINT('',(-1.19548183562566E-16,0.246528389340863,0.976185));
#8944=CARTESIAN_POINT('Origin',(-1.22464679914735E-16,0.,1.));
#8945=CARTESIAN_POINT('',(-0.976185,0.246528389340863,1.19548183562566E-16));
#8946=CARTESIAN_POINT('Origin',(0.,0.246528389340863,0.));
#8947=CARTESIAN_POINT('Origin',(0.,0.246528389340863,0.));
#8948=CARTESIAN_POINT('Origin',(0.,0.,0.));
#8949=CARTESIAN_POINT('',(-0.976185,0.45,-1.19548183562566E-16));
#8950=CARTESIAN_POINT('',(-0.976185,0.,-1.19548183562566E-16));
#8951=CARTESIAN_POINT('Origin',(0.,0.45,0.));
#8952=CARTESIAN_POINT('Origin',(0.,0.,0.));
#8953=CARTESIAN_POINT('',(-0.5,-0.39,-6.12323399573677E-17));
#8954=CARTESIAN_POINT('Origin',(0.,-0.39,0.));
#8955=CARTESIAN_POINT('',(-0.5,0.39,-6.12323399573677E-17));
#8956=CARTESIAN_POINT('',(-0.5,0.,-6.12323399573677E-17));
#8957=CARTESIAN_POINT('Origin',(0.,0.39,0.));
#8958=CARTESIAN_POINT('Origin',(0.,0.42,0.));
#8959=CARTESIAN_POINT('',(-0.56,0.45,-6.85802207522518E-17));
#8960=CARTESIAN_POINT('',(-0.53,0.42,-6.49062803548097E-17));
#8961=CARTESIAN_POINT('Origin',(0.,0.45,0.));
#8962=CARTESIAN_POINT('Origin',(0.976185,0.45,0.));
#8963=CARTESIAN_POINT('Origin',(0.,0.,0.));
#8964=CARTESIAN_POINT('',(-0.976185,-0.45,-1.19548183562566E-16));
#8965=CARTESIAN_POINT('Origin',(0.,-0.45,0.));
#8966=CARTESIAN_POINT('',(-0.976185,0.,-1.19548183562566E-16));
#8967=CARTESIAN_POINT('Origin',(0.56,-0.45,0.));
#8968=CARTESIAN_POINT('',(-0.56,-0.45,-6.85802207522518E-17));
#8969=CARTESIAN_POINT('Origin',(0.,-0.45,0.));
#8970=CARTESIAN_POINT('Origin',(0.,-0.42,0.));
#8971=CARTESIAN_POINT('',(-0.53,-0.42,-6.49062803548097E-17));
#8972=CARTESIAN_POINT('',(0.,0.,0.));
#8973=CARTESIAN_POINT('Origin',(0.,0.,0.));
#8974=CARTESIAN_POINT('',(-1.023815,0.246528389340863,-1.25381176266905E-16));
#8975=CARTESIAN_POINT('',(-1.25381176266905E-16,0.246528389340863,1.023815));
#8976=CARTESIAN_POINT('Origin',(0.,0.246528389340863,0.));
#8977=CARTESIAN_POINT('Origin',(0.,0.246528389340863,0.));
#8978=CARTESIAN_POINT('',(-1.25381176266905E-16,-0.246528389340863,1.023815));
#8979=CARTESIAN_POINT('Origin',(-1.22464679914735E-16,0.,1.));
#8980=CARTESIAN_POINT('',(-1.023815,-0.246528389340863,1.25381176266905E-16));
#8981=CARTESIAN_POINT('Origin',(0.,-0.246528389340863,0.));
#8982=CARTESIAN_POINT('Origin',(0.,-0.246528389340863,0.));
#8983=CARTESIAN_POINT('Origin',(0.,0.,0.));
#8984=CARTESIAN_POINT('',(-1.023815,-0.45,-1.25381176266905E-16));
#8985=CARTESIAN_POINT('Origin',(0.,-0.45,0.));
#8986=CARTESIAN_POINT('',(-1.023815,0.,-1.25381176266905E-16));
#8987=CARTESIAN_POINT('Origin',(1.44,0.45,0.));
#8988=CARTESIAN_POINT('',(-1.44,0.45,-1.76349139077219E-16));
#8989=CARTESIAN_POINT('Origin',(0.,0.45,0.));
#8990=CARTESIAN_POINT('',(-1.023815,0.45,-1.25381176266905E-16));
#8991=CARTESIAN_POINT('Origin',(0.,0.45,0.));
#8992=CARTESIAN_POINT('Origin',(0.,0.42,0.));
#8993=CARTESIAN_POINT('',(-1.5,0.39,-1.83697019872103E-16));
#8994=CARTESIAN_POINT('Origin',(0.,0.39,0.));
#8995=CARTESIAN_POINT('',(-1.47,0.42,-1.80023079474661E-16));
#8996=CARTESIAN_POINT('Origin',(0.,0.,0.));
#8997=CARTESIAN_POINT('',(-1.5,-0.39,-1.83697019872103E-16));
#8998=CARTESIAN_POINT('Origin',(0.,-0.39,0.));
#8999=CARTESIAN_POINT('',(-1.5,0.,-1.83697019872103E-16));
#9000=CARTESIAN_POINT('Origin',(0.,-0.42,0.));
#9001=CARTESIAN_POINT('',(-1.44,-0.45,-1.76349139077219E-16));
#9002=CARTESIAN_POINT('Origin',(0.,-0.45,0.));
#9003=CARTESIAN_POINT('',(-1.47,-0.42,-1.80023079474661E-16));
#9004=CARTESIAN_POINT('Origin',(1.023815,-0.45,0.));
#9005=CARTESIAN_POINT('Origin',(0.,0.,0.));
#9006=CARTESIAN_POINT('',(-1.023815,0.,-1.25381176266905E-16));
#9007=CARTESIAN_POINT('',(0.,0.,0.));
#9008=CARTESIAN_POINT('Origin',(1.,0.,0.));
#9009=CARTESIAN_POINT('',(1.,-1.78583896120461E-33,0.23815));
#9010=CARTESIAN_POINT('',(1.,-1.78583896120461E-33,-0.23815));
#9011=CARTESIAN_POINT('Origin',(1.,0.,0.));
#9012=CARTESIAN_POINT('Origin',(0.707106781186548,0.,-0.707106781186547));
#9013=CARTESIAN_POINT('',(0.875504261126124,-1.78583896120461E-33,-0.538709301246971));
#9014=CARTESIAN_POINT('',(0.538709301246971,-1.78583896120461E-33,-0.875504261126124));
#9015=CARTESIAN_POINT('Origin',(0.707106781186548,0.,-0.707106781186547));
#9016=CARTESIAN_POINT('Origin',(6.12323399573677E-17,0.,-1.));
#9017=CARTESIAN_POINT('',(0.23815,-1.78583896120461E-33,-1.));
#9018=CARTESIAN_POINT('',(-0.23815,-1.78583896120461E-33,-1.));
#9019=CARTESIAN_POINT('Origin',(6.12323399573677E-17,0.,-1.));
#9020=CARTESIAN_POINT('Origin',(-0.707106781186547,0.,-0.707106781186548));
#9021=CARTESIAN_POINT('',(-0.538709301246971,-1.78583896120461E-33,-0.875504261126124));
#9022=CARTESIAN_POINT('',(-0.875504261126124,-1.78583896120461E-33,-0.538709301246971));
#9023=CARTESIAN_POINT('Origin',(-0.707106781186547,0.,-0.707106781186548));
#9024=CARTESIAN_POINT('Origin',(-1.,0.,-1.22464679914735E-16));
#9025=CARTESIAN_POINT('',(-1.,-1.78583896120461E-33,-0.23815));
#9026=CARTESIAN_POINT('',(-1.,-1.78583896120461E-33,0.23815));
#9027=CARTESIAN_POINT('Origin',(-1.,0.,-1.22464679914735E-16));
#9028=CARTESIAN_POINT('Origin',(-0.707106781186548,0.,0.707106781186547));
#9029=CARTESIAN_POINT('',(-0.875504261126124,-7.94881478324376E-33,0.538709301246971));
#9030=CARTESIAN_POINT('',(-0.538709301246971,4.37713686083455E-33,0.875504261126124));
#9031=CARTESIAN_POINT('Origin',(-0.707106781186548,0.,0.707106781186547));
#9032=CARTESIAN_POINT('Origin',(-1.83697019872103E-16,0.,1.));
#9033=CARTESIAN_POINT('',(-0.23815,-1.78583896120461E-33,1.));
#9034=CARTESIAN_POINT('',(0.23815,-1.78583896120461E-33,1.));
#9035=CARTESIAN_POINT('Origin',(-1.83697019872103E-16,0.,1.));
#9036=CARTESIAN_POINT('Origin',(0.707106781186547,0.,0.707106781186548));
#9037=CARTESIAN_POINT('',(0.538709301246971,-4.86732687222419E-33,0.875504261126124));
#9038=CARTESIAN_POINT('',(0.875504261126124,1.29564894981497E-33,0.538709301246971));
#9039=CARTESIAN_POINT('Origin',(0.707106781186547,0.,0.707106781186548));
#9040=CARTESIAN_POINT('',(0.,0.,0.));
#9041=CARTESIAN_POINT('Origin',(0.707106781186547,0.,0.707106781186548));
#9042=CARTESIAN_POINT('',(0.504455939115715,-0.04763,0.841298510752802));
#9043=CARTESIAN_POINT('',(0.841298510752802,-0.04763,0.504455939115715));
#9044=CARTESIAN_POINT('Ctrl Pts',(0.504455939115715,-0.04763,0.841298510752802));
#9045=CARTESIAN_POINT('Ctrl Pts',(0.508899795931835,-0.0740444353928835,
0.838633903678357));
#9046=CARTESIAN_POINT('Ctrl Pts',(0.517157748491652,-0.0999305678883309,
0.833661031856294));
#9047=CARTESIAN_POINT('Ctrl Pts',(0.537715343527944,-0.142345102874864,
0.820511285096538));
#9048=CARTESIAN_POINT('Ctrl Pts',(0.548874290046456,-0.159766064500479,
0.813159949759));
#9049=CARTESIAN_POINT('Ctrl Pts',(0.573915184558107,-0.190326085855194,
0.795684265985089));
#9050=CARTESIAN_POINT('Ctrl Pts',(0.587792702767295,-0.203463743702801,
0.78555112003688));
#9051=CARTESIAN_POINT('Ctrl Pts',(0.615966552324775,-0.224161999508995,
0.763642258217233));
#9052=CARTESIAN_POINT('Ctrl Pts',(0.631684198665438,-0.232861760990032,
0.750785745543687));
#9053=CARTESIAN_POINT('Ctrl Pts',(0.663382628119203,-0.244251601209411,
0.722929908501543));
#9054=CARTESIAN_POINT('Ctrl Pts',(0.679352081686668,-0.246942143572133,
0.707917883896095));
#9055=CARTESIAN_POINT('Ctrl Pts',(0.707917883896095,-0.246942143572133,
0.679352081686668));
#9056=CARTESIAN_POINT('Ctrl Pts',(0.722929908501543,-0.244251601209411,
0.663382628119203));
#9057=CARTESIAN_POINT('Ctrl Pts',(0.750785745543687,-0.232861760990032,
0.631684198665439));
#9058=CARTESIAN_POINT('Ctrl Pts',(0.763642258217232,-0.224161999508995,
0.615966552324775));
#9059=CARTESIAN_POINT('Ctrl Pts',(0.78555112003688,-0.203463743702801,0.587792702767295));
#9060=CARTESIAN_POINT('Ctrl Pts',(0.795684265985088,-0.190326085855194,
0.573915184558108));
#9061=CARTESIAN_POINT('Ctrl Pts',(0.813159949759,-0.15976606450048,0.548874290046456));
#9062=CARTESIAN_POINT('Ctrl Pts',(0.820511285096538,-0.142345102874864,
0.537715343527944));
#9063=CARTESIAN_POINT('Ctrl Pts',(0.833661031856294,-0.099930567888331,
0.517157748491653));
#9064=CARTESIAN_POINT('Ctrl Pts',(0.838633903678357,-0.0740444353928835,
0.508899795931835));
#9065=CARTESIAN_POINT('Ctrl Pts',(0.841298510752801,-0.0476299999999999,
0.504455939115715));
#9066=CARTESIAN_POINT('',(0.528110872004958,-0.04763,0.871530771444223));
#9067=CARTESIAN_POINT('Origin',(0.707106781186547,-0.04763,0.707106781186548));
#9068=CARTESIAN_POINT('',(0.871530771444223,-0.04763,0.528110872004959));
#9069=CARTESIAN_POINT('Ctrl Pts',(0.871530771444223,-0.0476300000000001,
0.528110872004958));
#9070=CARTESIAN_POINT('Ctrl Pts',(0.87014664509073,-0.0609922781173483,
0.530395067942936));
#9071=CARTESIAN_POINT('Ctrl Pts',(0.868149331745851,-0.0742967091364493,
0.533674141594226));
#9072=CARTESIAN_POINT('Ctrl Pts',(0.85981294420286,-0.115492077056649,0.54708917182331));
#9073=CARTESIAN_POINT('Ctrl Pts',(0.850993704737257,-0.141695629206859,
0.560922177770136));
#9074=CARTESIAN_POINT('Ctrl Pts',(0.830754510485543,-0.181890537957859,
0.590422647829571));
#9075=CARTESIAN_POINT('Ctrl Pts',(0.816896541396381,-0.201072148666545,
0.609616703125488));
#9076=CARTESIAN_POINT('Ctrl Pts',(0.792310597819928,-0.223955109275652,
0.641117951819998));
#9077=CARTESIAN_POINT('Ctrl Pts',(0.779109323683612,-0.232742381310829,
0.657208095763053));
#9078=CARTESIAN_POINT('Ctrl Pts',(0.750552691816206,-0.244234834628584,
0.68964083160521));
#9079=CARTESIAN_POINT('Ctrl Pts',(0.735185187071673,-0.246942143572133,
0.705971972091755));
#9080=CARTESIAN_POINT('Ctrl Pts',(0.705971972091754,-0.246942143572133,
0.735185187071673));
#9081=CARTESIAN_POINT('Ctrl Pts',(0.689640831605209,-0.244234834628584,
0.750552691816206));
#9082=CARTESIAN_POINT('Ctrl Pts',(0.657208095763052,-0.232742381310829,
0.779109323683612));
#9083=CARTESIAN_POINT('Ctrl Pts',(0.641117951819998,-0.223955109275652,
0.792310597819928));
#9084=CARTESIAN_POINT('Ctrl Pts',(0.609616703125487,-0.201072148666545,
0.816896541396382));
#9085=CARTESIAN_POINT('Ctrl Pts',(0.590422647829571,-0.181890537957858,
0.830754510485544));
#9086=CARTESIAN_POINT('Ctrl Pts',(0.560922177770135,-0.141695629206858,
0.850993704737257));
#9087=CARTESIAN_POINT('Ctrl Pts',(0.547089171823309,-0.115492077056649,
0.859812944202861));
#9088=CARTESIAN_POINT('Ctrl Pts',(0.533674141594226,-0.0742967091364491,
0.868149331745852));
#9089=CARTESIAN_POINT('Ctrl Pts',(0.530395067942936,-0.0609922781173483,
0.870146645090731));
#9090=CARTESIAN_POINT('Ctrl Pts',(0.528110872004958,-0.0476300000000001,
0.871530771444223));
#9091=CARTESIAN_POINT('Origin',(0.707106781186547,-0.04763,0.707106781186548));
#9092=CARTESIAN_POINT('Origin',(0.,-0.166705,0.));
#9093=CARTESIAN_POINT('',(0.242834539687906,-0.04763,0.989696097314));
#9094=CARTESIAN_POINT('Origin',(0.,-0.04763,0.));
#9095=CARTESIAN_POINT('',(-0.242834539687907,-0.04763,0.989696097314));
#9096=CARTESIAN_POINT('Ctrl Pts',(0.242834539687906,-0.04763,0.989696097314));
#9097=CARTESIAN_POINT('Ctrl Pts',(0.24024064412003,-0.0609922781173483,
0.990332542620729));
#9098=CARTESIAN_POINT('Ctrl Pts',(0.236509675094874,-0.0742967091364492,
0.991238884025248));
#9099=CARTESIAN_POINT('Ctrl Pts',(0.221129100087819,-0.115492077056649,
0.994830026707808));
#9100=CARTESIAN_POINT('Ctrl Pts',(0.205111543747588,-0.141695629206859,
0.998375294985966));
#9101=CARTESIAN_POINT('Ctrl Pts',(0.169940289819232,-0.181890537957859,
1.00492400591205));
#9102=CARTESIAN_POINT('Ctrl Pts',(0.1465689792446,-0.201072148666545,1.00869718865384));
#9103=CARTESIAN_POINT('Ctrl Pts',(0.106909345252087,-0.223955109275652,
1.01358704779679));
#9104=CARTESIAN_POINT('Ctrl Pts',(0.0861971848975941,-0.232742381310829,
1.0156297872271));
#9105=CARTESIAN_POINT('Ctrl Pts',(0.0430711894098822,-0.244234834628584,
1.01837060663223));
#9106=CARTESIAN_POINT('Ctrl Pts',(0.0206568624125605,-0.246942143572133,
1.019052));
#9107=CARTESIAN_POINT('Ctrl Pts',(-0.0206568624125608,-0.246942143572133,
1.019052));
#9108=CARTESIAN_POINT('Ctrl Pts',(-0.0430711894098825,-0.244234834628584,
1.01837060663223));
#9109=CARTESIAN_POINT('Ctrl Pts',(-0.0861971848975943,-0.232742381310829,
1.0156297872271));
#9110=CARTESIAN_POINT('Ctrl Pts',(-0.106909345252088,-0.223955109275652,
1.01358704779679));
#9111=CARTESIAN_POINT('Ctrl Pts',(-0.1465689792446,-0.201072148666545,1.00869718865384));
#9112=CARTESIAN_POINT('Ctrl Pts',(-0.169940289819232,-0.181890537957859,
1.00492400591205));
#9113=CARTESIAN_POINT('Ctrl Pts',(-0.205111543747588,-0.141695629206859,
0.998375294985966));
#9114=CARTESIAN_POINT('Ctrl Pts',(-0.221129100087819,-0.115492077056649,
0.994830026707808));
#9115=CARTESIAN_POINT('Ctrl Pts',(-0.236509675094875,-0.0742967091364493,
0.991238884025248));
#9116=CARTESIAN_POINT('Ctrl Pts',(-0.24024064412003,-0.0609922781173483,
0.990332542620729));
#9117=CARTESIAN_POINT('Ctrl Pts',(-0.242834539687907,-0.04763,0.989696097314));
#9118=CARTESIAN_POINT('',(-0.528110872004959,-0.04763,0.871530771444223));
#9119=CARTESIAN_POINT('Origin',(0.,-0.04763,0.));
#9120=CARTESIAN_POINT('',(-0.871530771444223,-0.04763,0.528110872004958));
#9121=CARTESIAN_POINT('Ctrl Pts',(-0.528110872004958,-0.0476300000000001,
0.871530771444223));
#9122=CARTESIAN_POINT('Ctrl Pts',(-0.530395067942936,-0.0609922781173484,
0.87014664509073));
#9123=CARTESIAN_POINT('Ctrl Pts',(-0.533674141594226,-0.0742967091364493,
0.868149331745851));
#9124=CARTESIAN_POINT('Ctrl Pts',(-0.54708917182331,-0.115492077056649,
0.85981294420286));
#9125=CARTESIAN_POINT('Ctrl Pts',(-0.560922177770136,-0.141695629206859,
0.850993704737257));
#9126=CARTESIAN_POINT('Ctrl Pts',(-0.590422647829571,-0.181890537957859,
0.830754510485543));
#9127=CARTESIAN_POINT('Ctrl Pts',(-0.609616703125488,-0.201072148666545,
0.816896541396381));
#9128=CARTESIAN_POINT('Ctrl Pts',(-0.641117951819998,-0.223955109275652,
0.792310597819928));
#9129=CARTESIAN_POINT('Ctrl Pts',(-0.657208095763053,-0.232742381310829,
0.779109323683611));
#9130=CARTESIAN_POINT('Ctrl Pts',(-0.68964083160521,-0.244234834628584,
0.750552691816205));
#9131=CARTESIAN_POINT('Ctrl Pts',(-0.705971972091755,-0.246942143572133,
0.735185187071673));
#9132=CARTESIAN_POINT('Ctrl Pts',(-0.735185187071673,-0.246942143572133,
0.705971972091754));
#9133=CARTESIAN_POINT('Ctrl Pts',(-0.750552691816206,-0.244234834628584,
0.689640831605209));
#9134=CARTESIAN_POINT('Ctrl Pts',(-0.779109323683612,-0.232742381310829,
0.657208095763052));
#9135=CARTESIAN_POINT('Ctrl Pts',(-0.792310597819928,-0.223955109275652,
0.641117951819998));
#9136=CARTESIAN_POINT('Ctrl Pts',(-0.816896541396382,-0.201072148666545,
0.609616703125487));
#9137=CARTESIAN_POINT('Ctrl Pts',(-0.830754510485544,-0.181890537957858,
0.590422647829571));
#9138=CARTESIAN_POINT('Ctrl Pts',(-0.850993704737257,-0.141695629206858,
0.560922177770135));
#9139=CARTESIAN_POINT('Ctrl Pts',(-0.859812944202861,-0.115492077056649,
0.547089171823309));
#9140=CARTESIAN_POINT('Ctrl Pts',(-0.868149331745852,-0.0742967091364491,
0.533674141594226));
#9141=CARTESIAN_POINT('Ctrl Pts',(-0.870146645090731,-0.0609922781173483,
0.530395067942936));
#9142=CARTESIAN_POINT('Ctrl Pts',(-0.871530771444223,-0.04763,0.528110872004958));
#9143=CARTESIAN_POINT('',(-0.989696097314,-0.04763,0.242834539687906));
#9144=CARTESIAN_POINT('Origin',(0.,-0.04763,0.));
#9145=CARTESIAN_POINT('',(-1.019052,-0.246942143572133,1.248489836334E-16));
#9146=CARTESIAN_POINT('Ctrl Pts',(-0.989696097314,-0.04763,0.242834539687906));
#9147=CARTESIAN_POINT('Ctrl Pts',(-0.990332542620729,-0.0609922781173483,
0.24024064412003));
#9148=CARTESIAN_POINT('Ctrl Pts',(-0.991238884025248,-0.0742967091364492,
0.236509675094874));
#9149=CARTESIAN_POINT('Ctrl Pts',(-0.994830026707808,-0.115492077056649,
0.221129100087819));
#9150=CARTESIAN_POINT('Ctrl Pts',(-0.998375294985966,-0.141695629206859,
0.205111543747588));
#9151=CARTESIAN_POINT('Ctrl Pts',(-1.00492400591205,-0.181890537957859,
0.169940289819232));
#9152=CARTESIAN_POINT('Ctrl Pts',(-1.00869718865384,-0.201072148666545,
0.1465689792446));
#9153=CARTESIAN_POINT('Ctrl Pts',(-1.01358704779679,-0.223955109275652,
0.106909345252088));
#9154=CARTESIAN_POINT('Ctrl Pts',(-1.0156297872271,-0.232742381310829,0.0861971848975944));
#9155=CARTESIAN_POINT('Ctrl Pts',(-1.01837060663223,-0.244234834628584,
0.0430711894098825));
#9156=CARTESIAN_POINT('Ctrl Pts',(-1.019052,-0.246942143572133,0.0206568624125608));
#9157=CARTESIAN_POINT('Ctrl Pts',(-1.019052,-0.246942143572133,1.2490009027033E-16));
#9158=CARTESIAN_POINT('',(-1.019052,-0.28578,1.24797876996471E-16));
#9159=CARTESIAN_POINT('',(-1.019052,-0.166705,1.24797876996471E-16));
#9160=CARTESIAN_POINT('Origin',(0.,-0.28578,0.));
#9161=CARTESIAN_POINT('',(-0.989696097314,-0.04763,-0.242834539687906));
#9162=CARTESIAN_POINT('Ctrl Pts',(-1.019052,-0.246942143572133,1.2490009027033E-16));
#9163=CARTESIAN_POINT('Ctrl Pts',(-1.019052,-0.246942143572133,-0.0206568624125605));
#9164=CARTESIAN_POINT('Ctrl Pts',(-1.01837060663223,-0.244234834628584,
-0.0430711894098822));
#9165=CARTESIAN_POINT('Ctrl Pts',(-1.0156297872271,-0.232742381310829,-0.0861971848975941));
#9166=CARTESIAN_POINT('Ctrl Pts',(-1.01358704779679,-0.223955109275652,
-0.106909345252087));
#9167=CARTESIAN_POINT('Ctrl Pts',(-1.00869718865384,-0.201072148666546,
-0.1465689792446));
#9168=CARTESIAN_POINT('Ctrl Pts',(-1.00492400591205,-0.181890537957859,
-0.169940289819232));
#9169=CARTESIAN_POINT('Ctrl Pts',(-0.998375294985966,-0.141695629206859,
-0.205111543747588));
#9170=CARTESIAN_POINT('Ctrl Pts',(-0.994830026707808,-0.11549207705665,
-0.221129100087819));
#9171=CARTESIAN_POINT('Ctrl Pts',(-0.991238884025248,-0.0742967091364495,
-0.236509675094874));
#9172=CARTESIAN_POINT('Ctrl Pts',(-0.990332542620729,-0.0609922781173484,
-0.24024064412003));
#9173=CARTESIAN_POINT('Ctrl Pts',(-0.989696097314,-0.0476300000000001,-0.242834539687907));
#9174=CARTESIAN_POINT('',(-0.871530771444223,-0.04763,-0.528110872004958));
#9175=CARTESIAN_POINT('Origin',(0.,-0.04763,0.));
#9176=CARTESIAN_POINT('',(-0.528110872004958,-0.04763,-0.871530771444223));
#9177=CARTESIAN_POINT('Ctrl Pts',(-0.871530771444223,-0.0476300000000001,
-0.528110872004958));
#9178=CARTESIAN_POINT('Ctrl Pts',(-0.87014664509073,-0.0609922781173484,
-0.530395067942936));
#9179=CARTESIAN_POINT('Ctrl Pts',(-0.868149331745851,-0.0742967091364494,
-0.533674141594226));
#9180=CARTESIAN_POINT('Ctrl Pts',(-0.85981294420286,-0.115492077056649,
-0.54708917182331));
#9181=CARTESIAN_POINT('Ctrl Pts',(-0.850993704737257,-0.141695629206859,
-0.560922177770136));
#9182=CARTESIAN_POINT('Ctrl Pts',(-0.830754510485543,-0.181890537957859,
-0.590422647829571));
#9183=CARTESIAN_POINT('Ctrl Pts',(-0.816896541396381,-0.201072148666546,
-0.609616703125488));
#9184=CARTESIAN_POINT('Ctrl Pts',(-0.792310597819928,-0.223955109275652,
-0.641117951819999));
#9185=CARTESIAN_POINT('Ctrl Pts',(-0.779109323683611,-0.232742381310829,
-0.657208095763053));
#9186=CARTESIAN_POINT('Ctrl Pts',(-0.750552691816205,-0.244234834628584,
-0.68964083160521));
#9187=CARTESIAN_POINT('Ctrl Pts',(-0.735185187071673,-0.246942143572133,
-0.705971972091755));
#9188=CARTESIAN_POINT('Ctrl Pts',(-0.705971972091754,-0.246942143572133,
-0.735185187071673));
#9189=CARTESIAN_POINT('Ctrl Pts',(-0.68964083160521,-0.244234834628584,
-0.750552691816206));
#9190=CARTESIAN_POINT('Ctrl Pts',(-0.657208095763052,-0.232742381310829,
-0.779109323683612));
#9191=CARTESIAN_POINT('Ctrl Pts',(-0.641117951819998,-0.223955109275652,
-0.792310597819928));
#9192=CARTESIAN_POINT('Ctrl Pts',(-0.609616703125488,-0.201072148666545,
-0.816896541396381));
#9193=CARTESIAN_POINT('Ctrl Pts',(-0.590422647829571,-0.181890537957859,
-0.830754510485543));
#9194=CARTESIAN_POINT('Ctrl Pts',(-0.560922177770136,-0.141695629206859,
-0.850993704737257));
#9195=CARTESIAN_POINT('Ctrl Pts',(-0.54708917182331,-0.115492077056649,
-0.85981294420286));
#9196=CARTESIAN_POINT('Ctrl Pts',(-0.533674141594226,-0.0742967091364494,
-0.868149331745852));
#9197=CARTESIAN_POINT('Ctrl Pts',(-0.530395067942936,-0.0609922781173484,
-0.870146645090731));
#9198=CARTESIAN_POINT('Ctrl Pts',(-0.528110872004958,-0.0476300000000001,
-0.871530771444223));
#9199=CARTESIAN_POINT('',(-0.242834539687906,-0.04763,-0.989696097314));
#9200=CARTESIAN_POINT('Origin',(0.,-0.04763,0.));
#9201=CARTESIAN_POINT('',(0.242834539687906,-0.04763,-0.989696097314));
#9202=CARTESIAN_POINT('Ctrl Pts',(-0.242834539687907,-0.04763,-0.989696097314));
#9203=CARTESIAN_POINT('Ctrl Pts',(-0.24024064412003,-0.0609922781173483,
-0.990332542620729));
#9204=CARTESIAN_POINT('Ctrl Pts',(-0.236509675094874,-0.0742967091364493,
-0.991238884025248));
#9205=CARTESIAN_POINT('Ctrl Pts',(-0.221129100087819,-0.115492077056649,
-0.994830026707808));
#9206=CARTESIAN_POINT('Ctrl Pts',(-0.205111543747588,-0.141695629206859,
-0.998375294985966));
#9207=CARTESIAN_POINT('Ctrl Pts',(-0.169940289819232,-0.181890537957859,
-1.00492400591205));
#9208=CARTESIAN_POINT('Ctrl Pts',(-0.1465689792446,-0.201072148666545,-1.00869718865384));
#9209=CARTESIAN_POINT('Ctrl Pts',(-0.106909345252087,-0.223955109275652,
-1.01358704779679));
#9210=CARTESIAN_POINT('Ctrl Pts',(-0.0861971848975942,-0.232742381310829,
-1.0156297872271));
#9211=CARTESIAN_POINT('Ctrl Pts',(-0.0430711894098823,-0.244234834628584,
-1.01837060663223));
#9212=CARTESIAN_POINT('Ctrl Pts',(-0.0206568624125606,-0.246942143572133,
-1.019052));
#9213=CARTESIAN_POINT('Ctrl Pts',(0.0206568624125607,-0.246942143572133,
-1.019052));
#9214=CARTESIAN_POINT('Ctrl Pts',(0.0430711894098824,-0.244234834628584,
-1.01837060663223));
#9215=CARTESIAN_POINT('Ctrl Pts',(0.0861971848975943,-0.232742381310829,
-1.0156297872271));
#9216=CARTESIAN_POINT('Ctrl Pts',(0.106909345252088,-0.223955109275652,
-1.01358704779679));
#9217=CARTESIAN_POINT('Ctrl Pts',(0.1465689792446,-0.201072148666545,-1.00869718865384));
#9218=CARTESIAN_POINT('Ctrl Pts',(0.169940289819232,-0.181890537957859,
-1.00492400591205));
#9219=CARTESIAN_POINT('Ctrl Pts',(0.205111543747588,-0.141695629206859,
-0.998375294985966));
#9220=CARTESIAN_POINT('Ctrl Pts',(0.221129100087819,-0.115492077056649,
-0.994830026707808));
#9221=CARTESIAN_POINT('Ctrl Pts',(0.236509675094874,-0.0742967091364493,
-0.991238884025248));
#9222=CARTESIAN_POINT('Ctrl Pts',(0.24024064412003,-0.0609922781173484,
-0.990332542620729));
#9223=CARTESIAN_POINT('Ctrl Pts',(0.242834539687907,-0.04763,-0.989696097314));
#9224=CARTESIAN_POINT('',(0.528110872004958,-0.04763,-0.871530771444223));
#9225=CARTESIAN_POINT('Origin',(0.,-0.04763,0.));
#9226=CARTESIAN_POINT('',(0.871530771444223,-0.04763,-0.528110872004958));
#9227=CARTESIAN_POINT('Ctrl Pts',(0.528110872004958,-0.0476300000000001,
-0.871530771444223));
#9228=CARTESIAN_POINT('Ctrl Pts',(0.530395067942936,-0.0609922781173484,
-0.870146645090731));
#9229=CARTESIAN_POINT('Ctrl Pts',(0.533674141594226,-0.0742967091364493,
-0.868149331745851));
#9230=CARTESIAN_POINT('Ctrl Pts',(0.54708917182331,-0.115492077056649,-0.85981294420286));
#9231=CARTESIAN_POINT('Ctrl Pts',(0.560922177770136,-0.141695629206859,
-0.850993704737257));
#9232=CARTESIAN_POINT('Ctrl Pts',(0.590422647829571,-0.181890537957859,
-0.830754510485543));
#9233=CARTESIAN_POINT('Ctrl Pts',(0.609616703125488,-0.201072148666545,
-0.816896541396381));
#9234=CARTESIAN_POINT('Ctrl Pts',(0.641117951819998,-0.223955109275652,
-0.792310597819928));
#9235=CARTESIAN_POINT('Ctrl Pts',(0.657208095763053,-0.232742381310829,
-0.779109323683612));
#9236=CARTESIAN_POINT('Ctrl Pts',(0.68964083160521,-0.244234834628584,-0.750552691816206));
#9237=CARTESIAN_POINT('Ctrl Pts',(0.705971972091755,-0.246942143572133,
-0.735185187071673));
#9238=CARTESIAN_POINT('Ctrl Pts',(0.735185187071673,-0.246942143572133,
-0.705971972091754));
#9239=CARTESIAN_POINT('Ctrl Pts',(0.750552691816206,-0.244234834628584,
-0.68964083160521));
#9240=CARTESIAN_POINT('Ctrl Pts',(0.779109323683612,-0.232742381310829,
-0.657208095763053));
#9241=CARTESIAN_POINT('Ctrl Pts',(0.792310597819928,-0.223955109275652,
-0.641117951819998));
#9242=CARTESIAN_POINT('Ctrl Pts',(0.816896541396381,-0.201072148666545,
-0.609616703125488));
#9243=CARTESIAN_POINT('Ctrl Pts',(0.830754510485543,-0.181890537957859,
-0.590422647829571));
#9244=CARTESIAN_POINT('Ctrl Pts',(0.850993704737257,-0.141695629206859,
-0.560922177770136));
#9245=CARTESIAN_POINT('Ctrl Pts',(0.85981294420286,-0.115492077056649,-0.54708917182331));
#9246=CARTESIAN_POINT('Ctrl Pts',(0.868149331745851,-0.0742967091364493,
-0.533674141594226));
#9247=CARTESIAN_POINT('Ctrl Pts',(0.870146645090731,-0.0609922781173484,
-0.530395067942936));
#9248=CARTESIAN_POINT('Ctrl Pts',(0.871530771444223,-0.0476300000000001,
-0.528110872004958));
#9249=CARTESIAN_POINT('',(0.989696097314,-0.04763,-0.242834539687906));
#9250=CARTESIAN_POINT('Origin',(0.,-0.04763,0.));
#9251=CARTESIAN_POINT('',(0.989696097314,-0.04763,0.242834539687906));
#9252=CARTESIAN_POINT('Ctrl Pts',(0.989696097314,-0.04763,-0.242834539687907));
#9253=CARTESIAN_POINT('Ctrl Pts',(0.990332542620729,-0.0609922781173483,
-0.24024064412003));
#9254=CARTESIAN_POINT('Ctrl Pts',(0.991238884025248,-0.0742967091364493,
-0.236509675094874));
#9255=CARTESIAN_POINT('Ctrl Pts',(0.994830026707808,-0.115492077056649,
-0.221129100087819));
#9256=CARTESIAN_POINT('Ctrl Pts',(0.998375294985966,-0.141695629206859,
-0.205111543747588));
#9257=CARTESIAN_POINT('Ctrl Pts',(1.00492400591205,-0.181890537957859,-0.169940289819232));
#9258=CARTESIAN_POINT('Ctrl Pts',(1.00869718865384,-0.201072148666545,-0.1465689792446));
#9259=CARTESIAN_POINT('Ctrl Pts',(1.01358704779679,-0.223955109275652,-0.106909345252087));
#9260=CARTESIAN_POINT('Ctrl Pts',(1.0156297872271,-0.232742381310829,-0.0861971848975942));
#9261=CARTESIAN_POINT('Ctrl Pts',(1.01837060663223,-0.244234834628584,-0.0430711894098823));
#9262=CARTESIAN_POINT('Ctrl Pts',(1.019052,-0.246942143572133,-0.0206568624125607));
#9263=CARTESIAN_POINT('Ctrl Pts',(1.019052,-0.246942143572133,0.0206568624125607));
#9264=CARTESIAN_POINT('Ctrl Pts',(1.01837060663223,-0.244234834628584,0.0430711894098823));
#9265=CARTESIAN_POINT('Ctrl Pts',(1.0156297872271,-0.232742381310829,0.0861971848975942));
#9266=CARTESIAN_POINT('Ctrl Pts',(1.01358704779679,-0.223955109275652,0.106909345252087));
#9267=CARTESIAN_POINT('Ctrl Pts',(1.00869718865384,-0.201072148666545,0.1465689792446));
#9268=CARTESIAN_POINT('Ctrl Pts',(1.00492400591205,-0.181890537957859,0.169940289819232));
#9269=CARTESIAN_POINT('Ctrl Pts',(0.998375294985966,-0.141695629206859,
0.205111543747588));
#9270=CARTESIAN_POINT('Ctrl Pts',(0.994830026707808,-0.115492077056649,
0.221129100087819));
#9271=CARTESIAN_POINT('Ctrl Pts',(0.991238884025248,-0.0742967091364492,
0.236509675094874));
#9272=CARTESIAN_POINT('Ctrl Pts',(0.990332542620729,-0.0609922781173483,
0.24024064412003));
#9273=CARTESIAN_POINT('Ctrl Pts',(0.989696097314,-0.04763,0.242834539687907));
#9274=CARTESIAN_POINT('Origin',(0.,-0.04763,0.));
#9275=CARTESIAN_POINT('Origin',(0.,-0.04763,0.));
#9276=CARTESIAN_POINT('',(0.238183666596899,-0.04763,0.951592097314));
#9277=CARTESIAN_POINT('Origin',(0.,-0.04763,0.));
#9278=CARTESIAN_POINT('Origin',(-1.94289029309402E-16,-0.04763,1.));
#9279=CARTESIAN_POINT('Origin',(-1.94289029309402E-16,0.,1.));
#9280=CARTESIAN_POINT('',(-0.2381836665969,-0.04763,0.951592097314));
#9281=CARTESIAN_POINT('Ctrl Pts',(-0.238183666596899,-0.0476299999999999,
0.951592097314));
#9282=CARTESIAN_POINT('Ctrl Pts',(-0.233157223576062,-0.0740444353928835,
0.952850216871763));
#9283=CARTESIAN_POINT('Ctrl Pts',(-0.223801617934946,-0.0999305678883309,
0.955173119738174));
#9284=CARTESIAN_POINT('Ctrl Pts',(-0.199966927975188,-0.142345102874864,
0.960411259488514));
#9285=CARTESIAN_POINT('Ctrl Pts',(-0.1868781821531,-0.159766064500479,0.963103647174702));
#9286=CARTESIAN_POINT('Ctrl Pts',(-0.15681442133453,-0.190326085855194,
0.968453058988463));
#9287=CARTESIAN_POINT('Ctrl Pts',(-0.139836317888043,-0.203463743702801,
0.971100730005489));
#9288=CARTESIAN_POINT('Ctrl Pts',(-0.104422493053067,-0.224161999508995,
0.975530745318961));
#9289=CARTESIAN_POINT('Ctrl Pts',(-0.0842175114474176,-0.232861760990032,
0.977553872336861));
#9290=CARTESIAN_POINT('Ctrl Pts',(-0.0421062857595701,-0.244251601209411,
0.980270995488453));
#9291=CARTESIAN_POINT('Ctrl Pts',(-0.0201990724523197,-0.246942143572133,
0.980948));
#9292=CARTESIAN_POINT('Ctrl Pts',(0.020199072452319,-0.246942143572133,
0.980948));
#9293=CARTESIAN_POINT('Ctrl Pts',(0.0421062857595694,-0.244251601209411,
0.980270995488454));
#9294=CARTESIAN_POINT('Ctrl Pts',(0.0842175114474169,-0.232861760990032,
0.977553872336861));
#9295=CARTESIAN_POINT('Ctrl Pts',(0.104422493053067,-0.224161999508995,
0.975530745318961));
#9296=CARTESIAN_POINT('Ctrl Pts',(0.139836317888042,-0.203463743702801,
0.971100730005489));
#9297=CARTESIAN_POINT('Ctrl Pts',(0.15681442133453,-0.190326085855194,0.968453058988463));
#9298=CARTESIAN_POINT('Ctrl Pts',(0.1868781821531,-0.15976606450048,0.963103647174702));
#9299=CARTESIAN_POINT('Ctrl Pts',(0.199966927975188,-0.142345102874864,
0.960411259488514));
#9300=CARTESIAN_POINT('Ctrl Pts',(0.223801617934945,-0.0999305678883309,
0.955173119738174));
#9301=CARTESIAN_POINT('Ctrl Pts',(0.233157223576061,-0.0740444353928835,
0.952850216871763));
#9302=CARTESIAN_POINT('Ctrl Pts',(0.238183666596899,-0.0476299999999999,
0.951592097314));
#9303=CARTESIAN_POINT('Origin',(-1.94289029309402E-16,-0.04763,1.));
#9304=CARTESIAN_POINT('Origin',(0.,-0.04763,0.));
#9305=CARTESIAN_POINT('',(-0.504455939115715,-0.04763,0.841298510752802));
#9306=CARTESIAN_POINT('Origin',(0.,-0.04763,0.));
#9307=CARTESIAN_POINT('Origin',(-0.707106781186548,-0.04763,0.707106781186547));
#9308=CARTESIAN_POINT('Origin',(-0.707106781186548,0.,0.707106781186547));
#9309=CARTESIAN_POINT('',(-0.841298510752802,-0.04763,0.504455939115715));
#9310=CARTESIAN_POINT('Ctrl Pts',(-0.841298510752802,-0.04763,0.504455939115715));
#9311=CARTESIAN_POINT('Ctrl Pts',(-0.838633903678357,-0.0740444353928835,
0.508899795931835));
#9312=CARTESIAN_POINT('Ctrl Pts',(-0.833661031856294,-0.0999305678883309,
0.517157748491652));
#9313=CARTESIAN_POINT('Ctrl Pts',(-0.820511285096538,-0.142345102874864,
0.537715343527944));
#9314=CARTESIAN_POINT('Ctrl Pts',(-0.813159949759,-0.159766064500479,0.548874290046456));
#9315=CARTESIAN_POINT('Ctrl Pts',(-0.795684265985089,-0.190326085855194,
0.573915184558107));
#9316=CARTESIAN_POINT('Ctrl Pts',(-0.78555112003688,-0.203463743702801,
0.587792702767295));
#9317=CARTESIAN_POINT('Ctrl Pts',(-0.763642258217233,-0.224161999508995,
0.615966552324775));
#9318=CARTESIAN_POINT('Ctrl Pts',(-0.750785745543687,-0.232861760990032,
0.631684198665438));
#9319=CARTESIAN_POINT('Ctrl Pts',(-0.722929908501543,-0.244251601209411,
0.663382628119203));
#9320=CARTESIAN_POINT('Ctrl Pts',(-0.707917883896095,-0.246942143572133,
0.679352081686668));
#9321=CARTESIAN_POINT('Ctrl Pts',(-0.679352081686668,-0.246942143572133,
0.707917883896095));
#9322=CARTESIAN_POINT('Ctrl Pts',(-0.663382628119203,-0.244251601209411,
0.722929908501544));
#9323=CARTESIAN_POINT('Ctrl Pts',(-0.631684198665438,-0.232861760990031,
0.750785745543687));
#9324=CARTESIAN_POINT('Ctrl Pts',(-0.615966552324775,-0.224161999508995,
0.763642258217233));
#9325=CARTESIAN_POINT('Ctrl Pts',(-0.587792702767295,-0.203463743702801,
0.78555112003688));
#9326=CARTESIAN_POINT('Ctrl Pts',(-0.573915184558107,-0.190326085855194,
0.795684265985088));
#9327=CARTESIAN_POINT('Ctrl Pts',(-0.548874290046456,-0.159766064500479,
0.813159949759));
#9328=CARTESIAN_POINT('Ctrl Pts',(-0.537715343527944,-0.142345102874864,
0.820511285096538));
#9329=CARTESIAN_POINT('Ctrl Pts',(-0.517157748491652,-0.0999305678883309,
0.833661031856294));
#9330=CARTESIAN_POINT('Ctrl Pts',(-0.508899795931835,-0.0740444353928835,
0.838633903678357));
#9331=CARTESIAN_POINT('Ctrl Pts',(-0.504455939115716,-0.04763,0.841298510752801));
#9332=CARTESIAN_POINT('Origin',(-0.707106781186548,-0.04763,0.707106781186547));
#9333=CARTESIAN_POINT('Origin',(0.,-0.04763,0.));
#9334=CARTESIAN_POINT('',(-0.951592097314,-0.04763,0.238183666596899));
#9335=CARTESIAN_POINT('Origin',(0.,-0.04763,0.));
#9336=CARTESIAN_POINT('Origin',(-1.,-0.04763,-1.11022302462516E-16));
#9337=CARTESIAN_POINT('Origin',(-1.,0.,-1.11022302462516E-16));
#9338=CARTESIAN_POINT('',(-0.951592097314,-0.04763,-0.2381836665969));
#9339=CARTESIAN_POINT('',(-0.980948,-0.246942143572133,1.08514323328844E-18));
#9340=CARTESIAN_POINT('Ctrl Pts',(-0.951592097314,-0.04763,-0.238183666596899));
#9341=CARTESIAN_POINT('Ctrl Pts',(-0.952850216871763,-0.0740444353928835,
-0.233157223576062));
#9342=CARTESIAN_POINT('Ctrl Pts',(-0.955173119738174,-0.0999305678883309,
-0.223801617934946));
#9343=CARTESIAN_POINT('Ctrl Pts',(-0.960411259488514,-0.142345102874864,
-0.199966927975188));
#9344=CARTESIAN_POINT('Ctrl Pts',(-0.963103647174702,-0.159766064500479,
-0.1868781821531));
#9345=CARTESIAN_POINT('Ctrl Pts',(-0.968453058988463,-0.190326085855194,
-0.15681442133453));
#9346=CARTESIAN_POINT('Ctrl Pts',(-0.971100730005489,-0.203463743702801,
-0.139836317888043));
#9347=CARTESIAN_POINT('Ctrl Pts',(-0.975530745318961,-0.224161999508995,
-0.104422493053067));
#9348=CARTESIAN_POINT('Ctrl Pts',(-0.977553872336861,-0.232861760990032,
-0.0842175114474175));
#9349=CARTESIAN_POINT('Ctrl Pts',(-0.980270995488453,-0.244251601209411,
-0.0421062857595699));
#9350=CARTESIAN_POINT('Ctrl Pts',(-0.980948,-0.246942143572133,-0.0201990724523195));
#9351=CARTESIAN_POINT('Ctrl Pts',(-0.980948,-0.246942143572133,-1.17961196366423E-16));
#9352=CARTESIAN_POINT('Origin',(-1.,-0.04763,-1.11022302462516E-16));
#9353=CARTESIAN_POINT('Ctrl Pts',(-0.980948,-0.246942143572133,-1.17961196366423E-16));
#9354=CARTESIAN_POINT('Ctrl Pts',(-0.980948,-0.246942143572133,0.0201990724523192));
#9355=CARTESIAN_POINT('Ctrl Pts',(-0.980270995488453,-0.244251601209411,
0.0421062857595695));
#9356=CARTESIAN_POINT('Ctrl Pts',(-0.977553872336861,-0.232861760990032,
0.0842175114474169));
#9357=CARTESIAN_POINT('Ctrl Pts',(-0.975530745318961,-0.224161999508995,
0.104422493053066));
#9358=CARTESIAN_POINT('Ctrl Pts',(-0.971100730005489,-0.203463743702801,
0.139836317888042));
#9359=CARTESIAN_POINT('Ctrl Pts',(-0.968453058988463,-0.190326085855194,
0.15681442133453));
#9360=CARTESIAN_POINT('Ctrl Pts',(-0.963103647174702,-0.15976606450048,
0.1868781821531));
#9361=CARTESIAN_POINT('Ctrl Pts',(-0.960411259488514,-0.142345102874864,
0.199966927975188));
#9362=CARTESIAN_POINT('Ctrl Pts',(-0.955173119738174,-0.099930567888331,
0.223801617934945));
#9363=CARTESIAN_POINT('Ctrl Pts',(-0.952850216871763,-0.0740444353928835,
0.233157223576061));
#9364=CARTESIAN_POINT('Ctrl Pts',(-0.951592097314,-0.04763,0.238183666596899));
#9365=CARTESIAN_POINT('Origin',(0.,-0.04763,0.));
#9366=CARTESIAN_POINT('',(-0.841298510752802,-0.04763,-0.504455939115715));
#9367=CARTESIAN_POINT('Origin',(0.,-0.04763,0.));
#9368=CARTESIAN_POINT('Origin',(-0.707106781186547,-0.04763,-0.707106781186548));
#9369=CARTESIAN_POINT('Origin',(-0.707106781186547,0.,-0.707106781186548));
#9370=CARTESIAN_POINT('',(-0.504455939115715,-0.04763,-0.841298510752802));
#9371=CARTESIAN_POINT('Ctrl Pts',(-0.504455939115715,-0.04763,-0.841298510752802));
#9372=CARTESIAN_POINT('Ctrl Pts',(-0.508899795931835,-0.0740444353928835,
-0.838633903678357));
#9373=CARTESIAN_POINT('Ctrl Pts',(-0.517157748491652,-0.0999305678883309,
-0.833661031856294));
#9374=CARTESIAN_POINT('Ctrl Pts',(-0.537715343527944,-0.142345102874864,
-0.820511285096538));
#9375=CARTESIAN_POINT('Ctrl Pts',(-0.548874290046456,-0.159766064500479,
-0.813159949759));
#9376=CARTESIAN_POINT('Ctrl Pts',(-0.573915184558107,-0.190326085855194,
-0.795684265985089));
#9377=CARTESIAN_POINT('Ctrl Pts',(-0.587792702767295,-0.203463743702801,
-0.78555112003688));
#9378=CARTESIAN_POINT('Ctrl Pts',(-0.615966552324775,-0.224161999508995,
-0.763642258217233));
#9379=CARTESIAN_POINT('Ctrl Pts',(-0.631684198665438,-0.232861760990032,
-0.750785745543687));
#9380=CARTESIAN_POINT('Ctrl Pts',(-0.663382628119203,-0.244251601209411,
-0.722929908501543));
#9381=CARTESIAN_POINT('Ctrl Pts',(-0.679352081686668,-0.246942143572133,
-0.707917883896095));
#9382=CARTESIAN_POINT('Ctrl Pts',(-0.707917883896095,-0.246942143572133,
-0.679352081686668));
#9383=CARTESIAN_POINT('Ctrl Pts',(-0.722929908501543,-0.244251601209411,
-0.663382628119203));
#9384=CARTESIAN_POINT('Ctrl Pts',(-0.750785745543687,-0.232861760990032,
-0.631684198665439));
#9385=CARTESIAN_POINT('Ctrl Pts',(-0.763642258217232,-0.224161999508995,
-0.615966552324775));
#9386=CARTESIAN_POINT('Ctrl Pts',(-0.78555112003688,-0.203463743702801,
-0.587792702767295));
#9387=CARTESIAN_POINT('Ctrl Pts',(-0.795684265985088,-0.190326085855194,
-0.573915184558107));
#9388=CARTESIAN_POINT('Ctrl Pts',(-0.813159949759,-0.15976606450048,-0.548874290046456));
#9389=CARTESIAN_POINT('Ctrl Pts',(-0.820511285096538,-0.142345102874864,
-0.537715343527944));
#9390=CARTESIAN_POINT('Ctrl Pts',(-0.833661031856294,-0.0999305678883311,
-0.517157748491652));
#9391=CARTESIAN_POINT('Ctrl Pts',(-0.838633903678357,-0.0740444353928836,
-0.508899795931835));
#9392=CARTESIAN_POINT('Ctrl Pts',(-0.841298510752801,-0.04763,-0.504455939115715));
#9393=CARTESIAN_POINT('Origin',(-0.707106781186547,-0.04763,-0.707106781186548));
#9394=CARTESIAN_POINT('Origin',(0.,-0.04763,0.));
#9395=CARTESIAN_POINT('',(-0.238183666596899,-0.04763,-0.951592097314));
#9396=CARTESIAN_POINT('Origin',(0.,-0.04763,0.));
#9397=CARTESIAN_POINT('Origin',(5.55111512312578E-17,-0.04763,-1.));
#9398=CARTESIAN_POINT('Origin',(5.55111512312578E-17,0.,-1.));
#9399=CARTESIAN_POINT('',(0.238183666596899,-0.04763,-0.951592097314));
#9400=CARTESIAN_POINT('Ctrl Pts',(0.238183666596899,-0.04763,-0.951592097314));
#9401=CARTESIAN_POINT('Ctrl Pts',(0.233157223576062,-0.0740444353928835,
-0.952850216871763));
#9402=CARTESIAN_POINT('Ctrl Pts',(0.223801617934946,-0.099930567888331,
-0.955173119738174));
#9403=CARTESIAN_POINT('Ctrl Pts',(0.199966927975188,-0.142345102874864,
-0.960411259488514));
#9404=CARTESIAN_POINT('Ctrl Pts',(0.1868781821531,-0.15976606450048,-0.963103647174702));
#9405=CARTESIAN_POINT('Ctrl Pts',(0.15681442133453,-0.190326085855194,-0.968453058988463));
#9406=CARTESIAN_POINT('Ctrl Pts',(0.139836317888042,-0.203463743702801,
-0.971100730005489));
#9407=CARTESIAN_POINT('Ctrl Pts',(0.104422493053067,-0.224161999508995,
-0.975530745318961));
#9408=CARTESIAN_POINT('Ctrl Pts',(0.0842175114474173,-0.232861760990032,
-0.977553872336861));
#9409=CARTESIAN_POINT('Ctrl Pts',(0.0421062857595698,-0.244251601209411,
-0.980270995488453));
#9410=CARTESIAN_POINT('Ctrl Pts',(0.0201990724523194,-0.246942143572133,
-0.980948));
#9411=CARTESIAN_POINT('Ctrl Pts',(-0.0201990724523193,-0.246942143572133,
-0.980948));
#9412=CARTESIAN_POINT('Ctrl Pts',(-0.0421062857595697,-0.244251601209411,
-0.980270995488453));
#9413=CARTESIAN_POINT('Ctrl Pts',(-0.0842175114474171,-0.232861760990032,
-0.977553872336861));
#9414=CARTESIAN_POINT('Ctrl Pts',(-0.104422493053067,-0.224161999508995,
-0.975530745318961));
#9415=CARTESIAN_POINT('Ctrl Pts',(-0.139836317888042,-0.203463743702801,
-0.971100730005489));
#9416=CARTESIAN_POINT('Ctrl Pts',(-0.15681442133453,-0.190326085855194,
-0.968453058988463));
#9417=CARTESIAN_POINT('Ctrl Pts',(-0.1868781821531,-0.15976606450048,-0.963103647174702));
#9418=CARTESIAN_POINT('Ctrl Pts',(-0.199966927975188,-0.142345102874864,
-0.960411259488514));
#9419=CARTESIAN_POINT('Ctrl Pts',(-0.223801617934945,-0.099930567888331,
-0.955173119738174));
#9420=CARTESIAN_POINT('Ctrl Pts',(-0.233157223576062,-0.0740444353928835,
-0.952850216871763));
#9421=CARTESIAN_POINT('Ctrl Pts',(-0.238183666596899,-0.0476299999999999,
-0.951592097314));
#9422=CARTESIAN_POINT('Origin',(5.55111512312578E-17,-0.04763,-1.));
#9423=CARTESIAN_POINT('Origin',(0.,-0.04763,0.));
#9424=CARTESIAN_POINT('',(0.504455939115715,-0.04763,-0.841298510752802));
#9425=CARTESIAN_POINT('Origin',(0.,-0.04763,0.));
#9426=CARTESIAN_POINT('Origin',(0.707106781186548,-0.04763,-0.707106781186547));
#9427=CARTESIAN_POINT('Origin',(0.707106781186548,0.,-0.707106781186547));
#9428=CARTESIAN_POINT('',(0.841298510752802,-0.04763,-0.504455939115715));
#9429=CARTESIAN_POINT('Ctrl Pts',(0.841298510752802,-0.04763,-0.504455939115715));
#9430=CARTESIAN_POINT('Ctrl Pts',(0.838633903678357,-0.0740444353928835,
-0.508899795931835));
#9431=CARTESIAN_POINT('Ctrl Pts',(0.833661031856294,-0.0999305678883309,
-0.517157748491652));
#9432=CARTESIAN_POINT('Ctrl Pts',(0.820511285096538,-0.142345102874864,
-0.537715343527944));
#9433=CARTESIAN_POINT('Ctrl Pts',(0.813159949759,-0.159766064500479,-0.548874290046456));
#9434=CARTESIAN_POINT('Ctrl Pts',(0.795684265985088,-0.190326085855194,
-0.573915184558107));
#9435=CARTESIAN_POINT('Ctrl Pts',(0.78555112003688,-0.203463743702801,-0.587792702767295));
#9436=CARTESIAN_POINT('Ctrl Pts',(0.763642258217233,-0.224161999508995,
-0.615966552324775));
#9437=CARTESIAN_POINT('Ctrl Pts',(0.750785745543687,-0.232861760990032,
-0.631684198665438));
#9438=CARTESIAN_POINT('Ctrl Pts',(0.722929908501543,-0.244251601209411,
-0.663382628119203));
#9439=CARTESIAN_POINT('Ctrl Pts',(0.707917883896095,-0.246942143572133,
-0.679352081686668));
#9440=CARTESIAN_POINT('Ctrl Pts',(0.679352081686668,-0.246942143572133,
-0.707917883896095));
#9441=CARTESIAN_POINT('Ctrl Pts',(0.663382628119203,-0.244251601209411,
-0.722929908501543));
#9442=CARTESIAN_POINT('Ctrl Pts',(0.631684198665438,-0.232861760990032,
-0.750785745543687));
#9443=CARTESIAN_POINT('Ctrl Pts',(0.615966552324775,-0.224161999508995,
-0.763642258217232));
#9444=CARTESIAN_POINT('Ctrl Pts',(0.587792702767295,-0.203463743702801,
-0.78555112003688));
#9445=CARTESIAN_POINT('Ctrl Pts',(0.573915184558107,-0.190326085855194,
-0.795684265985088));
#9446=CARTESIAN_POINT('Ctrl Pts',(0.548874290046456,-0.159766064500479,
-0.813159949759));
#9447=CARTESIAN_POINT('Ctrl Pts',(0.537715343527944,-0.142345102874864,
-0.820511285096538));
#9448=CARTESIAN_POINT('Ctrl Pts',(0.517157748491652,-0.099930567888331,
-0.833661031856294));
#9449=CARTESIAN_POINT('Ctrl Pts',(0.508899795931835,-0.0740444353928835,
-0.838633903678357));
#9450=CARTESIAN_POINT('Ctrl Pts',(0.504455939115715,-0.04763,-0.841298510752801));
#9451=CARTESIAN_POINT('Origin',(0.707106781186548,-0.04763,-0.707106781186547));
#9452=CARTESIAN_POINT('Origin',(0.,-0.166705,0.));
#9453=CARTESIAN_POINT('',(-0.980948,-0.28578,1.20131482833E-16));
#9454=CARTESIAN_POINT('Origin',(0.,-0.28578,0.));
#9455=CARTESIAN_POINT('',(-0.980948,-0.166705,1.20131482833E-16));
#9456=CARTESIAN_POINT('',(0.951592097314,-0.04763,0.238183666596899));
#9457=CARTESIAN_POINT('Origin',(0.,-0.04763,0.));
#9458=CARTESIAN_POINT('',(0.951592097314,-0.04763,-0.238183666596899));
#9459=CARTESIAN_POINT('Ctrl Pts',(0.951592097314,-0.04763,0.238183666596899));
#9460=CARTESIAN_POINT('Ctrl Pts',(0.952850216871763,-0.0740444353928835,
0.233157223576062));
#9461=CARTESIAN_POINT('Ctrl Pts',(0.955173119738174,-0.099930567888331,
0.223801617934945));
#9462=CARTESIAN_POINT('Ctrl Pts',(0.960411259488514,-0.142345102874864,
0.199966927975188));
#9463=CARTESIAN_POINT('Ctrl Pts',(0.963103647174702,-0.15976606450048,0.1868781821531));
#9464=CARTESIAN_POINT('Ctrl Pts',(0.968453058988463,-0.190326085855194,
0.15681442133453));
#9465=CARTESIAN_POINT('Ctrl Pts',(0.971100730005489,-0.203463743702801,
0.139836317888042));
#9466=CARTESIAN_POINT('Ctrl Pts',(0.975530745318961,-0.224161999508995,
0.104422493053067));
#9467=CARTESIAN_POINT('Ctrl Pts',(0.977553872336861,-0.232861760990032,
0.0842175114474172));
#9468=CARTESIAN_POINT('Ctrl Pts',(0.980270995488453,-0.244251601209411,
0.0421062857595697));
#9469=CARTESIAN_POINT('Ctrl Pts',(0.980948,-0.246942143572133,0.0201990724523194));
#9470=CARTESIAN_POINT('Ctrl Pts',(0.980948,-0.246942143572133,-0.0201990724523194));
#9471=CARTESIAN_POINT('Ctrl Pts',(0.980270995488453,-0.244251601209411,
-0.0421062857595697));
#9472=CARTESIAN_POINT('Ctrl Pts',(0.977553872336861,-0.232861760990032,
-0.0842175114474172));
#9473=CARTESIAN_POINT('Ctrl Pts',(0.975530745318961,-0.224161999508995,
-0.104422493053067));
#9474=CARTESIAN_POINT('Ctrl Pts',(0.971100730005489,-0.203463743702801,
-0.139836317888042));
#9475=CARTESIAN_POINT('Ctrl Pts',(0.968453058988463,-0.190326085855194,
-0.15681442133453));
#9476=CARTESIAN_POINT('Ctrl Pts',(0.963103647174702,-0.15976606450048,-0.1868781821531));
#9477=CARTESIAN_POINT('Ctrl Pts',(0.960411259488514,-0.142345102874864,
-0.199966927975188));
#9478=CARTESIAN_POINT('Ctrl Pts',(0.955173119738174,-0.099930567888331,
-0.223801617934945));
#9479=CARTESIAN_POINT('Ctrl Pts',(0.952850216871763,-0.0740444353928835,
-0.233157223576062));
#9480=CARTESIAN_POINT('Ctrl Pts',(0.951592097314,-0.0476299999999999,-0.238183666596899));
#9481=CARTESIAN_POINT('Origin',(0.,-0.04763,0.));
#9482=CARTESIAN_POINT('Origin',(0.,-0.04763,0.));
#9483=CARTESIAN_POINT('Origin',(1.,-0.04763,0.));
#9484=CARTESIAN_POINT('Origin',(1.,0.,0.));
#9485=CARTESIAN_POINT('Origin',(1.,-0.04763,0.));
#9486=CARTESIAN_POINT('Origin',(0.,-0.28578,0.));
#9487=CARTESIAN_POINT('Origin',(0.,-0.04763,0.));
#9488=CARTESIAN_POINT('',(0.,0.,0.));
#9489=CARTESIAN_POINT('Origin',(1.013815,0.445,0.));
#9490=CARTESIAN_POINT('',(-1.013815,0.445,-1.24156529467757E-16));
#9491=CARTESIAN_POINT('Origin',(0.,0.445,0.));
#9492=CARTESIAN_POINT('',(-0.991185,0.445,-1.21385153761287E-16));
#9493=CARTESIAN_POINT('Origin',(0.,0.445,0.));
#9494=CARTESIAN_POINT('Origin',(0.,0.4075,0.));
#9495=CARTESIAN_POINT('',(-1.013815,0.37,-1.24156529467757E-16));
#9496=CARTESIAN_POINT('Origin',(0.,0.37,0.));
#9497=CARTESIAN_POINT('',(-1.013815,0.4075,-1.24156529467757E-16));
#9498=CARTESIAN_POINT('Origin',(0.991185,0.37,0.));
#9499=CARTESIAN_POINT('',(-0.991185,0.37,-1.21385153761287E-16));
#9500=CARTESIAN_POINT('Origin',(0.,0.37,0.));
#9501=CARTESIAN_POINT('Origin',(0.,0.4075,0.));
#9502=CARTESIAN_POINT('',(-0.991185,0.4075,-1.21385153761287E-16));
#9503=CARTESIAN_POINT('Origin',(1.013815,-0.37,0.));
#9504=CARTESIAN_POINT('',(-1.013815,-0.37,-1.24156529467757E-16));
#9505=CARTESIAN_POINT('Origin',(0.,-0.37,0.));
#9506=CARTESIAN_POINT('',(-0.991185,-0.37,-1.21385153761287E-16));
#9507=CARTESIAN_POINT('Origin',(0.,-0.37,0.));
#9508=CARTESIAN_POINT('Origin',(0.,-0.4075,0.));
#9509=CARTESIAN_POINT('',(-1.013815,-0.445,-1.24156529467757E-16));
#9510=CARTESIAN_POINT('Origin',(0.,-0.445,0.));
#9511=CARTESIAN_POINT('',(-1.013815,-0.4075,-1.24156529467757E-16));
#9512=CARTESIAN_POINT('Origin',(0.991185,-0.445,0.));
#9513=CARTESIAN_POINT('',(-0.991185,-0.445,-1.21385153761287E-16));
#9514=CARTESIAN_POINT('Origin',(0.,-0.445,0.));
#9515=CARTESIAN_POINT('Origin',(0.,-0.4075,0.));
#9516=CARTESIAN_POINT('',(-0.991185,-0.4075,-1.21385153761287E-16));
#9517=CARTESIAN_POINT('',(0.,0.,0.));
#9518=CARTESIAN_POINT('',(0.,0.,0.));
#9519=CARTESIAN_POINT('',(0.,0.,0.));
#9520=CARTESIAN_POINT('',(0.,0.,0.));
#9521=CARTESIAN_POINT('',(0.,0.,0.));
#9522=CARTESIAN_POINT('',(0.,0.,0.));
#9523=CARTESIAN_POINT('Origin',(8.,0.,0.));
#9524=CARTESIAN_POINT('',(8.,7.34788079488412E-17,0.6));
#9525=CARTESIAN_POINT('Origin',(8.,0.,0.));
#9526=CARTESIAN_POINT('Origin',(0.05,0.,0.));
#9527=CARTESIAN_POINT('',(0.1,7.34788079488412E-17,0.6));
#9528=CARTESIAN_POINT('Origin',(0.1,0.,0.));
#9529=CARTESIAN_POINT('',(0.,-6.12323399573677E-17,0.5));
#9530=CARTESIAN_POINT('',(0.05,-6.73555739531044E-17,0.55));
#9531=CARTESIAN_POINT('Origin',(0.,0.,0.));
#9532=CARTESIAN_POINT('Origin',(0.,0.,0.));
#9533=CARTESIAN_POINT('',(0.,-7.34788079488412E-17,0.6));
#9534=CARTESIAN_POINT('Origin',(0.,0.,0.));
#9535=CARTESIAN_POINT('',(0.,0.,0.));
#9536=CARTESIAN_POINT('Origin',(6.,3.7,1.));
#9537=CARTESIAN_POINT('',(6.,3.7,1.));
#9538=CARTESIAN_POINT('',(5.,3.7,1.));
#9539=CARTESIAN_POINT('',(6.,3.7,1.));
#9540=CARTESIAN_POINT('',(5.,3.7,5.));
#9541=CARTESIAN_POINT('',(5.,3.7,1.));
#9542=CARTESIAN_POINT('',(6.,3.7,5.));
#9543=CARTESIAN_POINT('',(6.,3.7,5.));
#9544=CARTESIAN_POINT('',(6.,3.7,1.));
#9545=CARTESIAN_POINT('Origin',(5.,0.3,1.));
#9546=CARTESIAN_POINT('',(5.,0.3,1.));
#9547=CARTESIAN_POINT('',(6.,0.3,1.));
#9548=CARTESIAN_POINT('',(5.,0.3,1.));
#9549=CARTESIAN_POINT('',(6.,0.3,5.));
#9550=CARTESIAN_POINT('',(6.,0.3,1.));
#9551=CARTESIAN_POINT('',(5.,0.3,5.));
#9552=CARTESIAN_POINT('',(5.,0.3,5.));
#9553=CARTESIAN_POINT('',(5.,0.3,1.));
#9554=CARTESIAN_POINT('Origin',(5.5,2.,4.59));
#9555=CARTESIAN_POINT('',(5.3762058159686,1.89091287885364,4.59));
#9556=CARTESIAN_POINT('',(5.6237941840314,1.89091287885364,4.59));
#9557=CARTESIAN_POINT('',(4.9,1.89091287885364,4.59));
#9558=CARTESIAN_POINT('Origin',(5.5,2.,4.59));
#9559=CARTESIAN_POINT('Origin',(5.5,2.,4.59));
#9560=CARTESIAN_POINT('',(5.3762058159686,2.10908712114636,4.59));
#9561=CARTESIAN_POINT('',(5.335,2.,4.6));
#9562=CARTESIAN_POINT('Ctrl Pts',(5.3762058159686,2.10908712114636,4.59));
#9563=CARTESIAN_POINT('Ctrl Pts',(5.36460086481047,2.09591759715261,4.59243495840567));
#9564=CARTESIAN_POINT('Ctrl Pts',(5.35465435634175,2.08022344943772,4.59485638705045));
#9565=CARTESIAN_POINT('Ctrl Pts',(5.33918513536598,2.04298016596019,4.59880705606552));
#9566=CARTESIAN_POINT('Ctrl Pts',(5.335,2.02083185350888,4.6));
#9567=CARTESIAN_POINT('Ctrl Pts',(5.335,2.,4.6));
#9568=CARTESIAN_POINT('',(5.6237941840314,2.10908712114636,4.59));
#9569=CARTESIAN_POINT('Origin',(5.5,2.,4.59));
#9570=CARTESIAN_POINT('',(5.665,2.,4.6));
#9571=CARTESIAN_POINT('Ctrl Pts',(5.665,2.,4.6));
#9572=CARTESIAN_POINT('Ctrl Pts',(5.665,2.02083185350888,4.6));
#9573=CARTESIAN_POINT('Ctrl Pts',(5.66081486463402,2.04298016596019,4.59880705606552));
#9574=CARTESIAN_POINT('Ctrl Pts',(5.64534564365825,2.08022344943772,4.59485638705045));
#9575=CARTESIAN_POINT('Ctrl Pts',(5.63539913518953,2.09591759715261,4.59243495840567));
#9576=CARTESIAN_POINT('Ctrl Pts',(5.6237941840314,2.10908712114636,4.59));
#9577=CARTESIAN_POINT('Ctrl Pts',(5.6237941840314,1.89091287885364,4.59));
#9578=CARTESIAN_POINT('Ctrl Pts',(5.63539913518953,1.90408240284739,4.59243495840567));
#9579=CARTESIAN_POINT('Ctrl Pts',(5.64534564365825,1.91977655056228,4.59485638705045));
#9580=CARTESIAN_POINT('Ctrl Pts',(5.66081486463402,1.95701983403981,4.59880705606552));
#9581=CARTESIAN_POINT('Ctrl Pts',(5.665,1.97916814649112,4.6));
#9582=CARTESIAN_POINT('Ctrl Pts',(5.665,2.,4.6));
#9583=CARTESIAN_POINT('Ctrl Pts',(5.335,2.,4.6));
#9584=CARTESIAN_POINT('Ctrl Pts',(5.335,1.97916814649112,4.6));
#9585=CARTESIAN_POINT('Ctrl Pts',(5.33918513536598,1.95701983403981,4.59880705606552));
#9586=CARTESIAN_POINT('Ctrl Pts',(5.35465435634175,1.91977655056228,4.59485638705045));
#9587=CARTESIAN_POINT('Ctrl Pts',(5.36460086481047,1.90408240284739,4.59243495840567));
#9588=CARTESIAN_POINT('Ctrl Pts',(5.3762058159686,1.89091287885364,4.59));
#9589=CARTESIAN_POINT('',(5.335,2.,5.));
#9590=CARTESIAN_POINT('',(5.335,2.,4.59));
#9591=CARTESIAN_POINT('Origin',(5.5,2.,5.));
#9592=CARTESIAN_POINT('Origin',(5.5,2.,4.59));
#9593=CARTESIAN_POINT('',(4.9,2.10908712114636,4.59));
#9594=CARTESIAN_POINT('Origin',(5.5,0.9,2.));
#9595=CARTESIAN_POINT('',(5.1,0.9,2.));
#9596=CARTESIAN_POINT('Origin',(5.5,0.9,2.));
#9597=CARTESIAN_POINT('',(5.1,0.9,5.));
#9598=CARTESIAN_POINT('',(5.1,0.9,2.));
#9599=CARTESIAN_POINT('Origin',(5.5,0.9,5.));
#9600=CARTESIAN_POINT('Origin',(5.5,0.9,2.));
#9601=CARTESIAN_POINT('',(5.275,0.9,2.));
#9602=CARTESIAN_POINT('Origin',(5.5,0.9,2.));
#9603=CARTESIAN_POINT('Origin',(5.5,3.1,2.));
#9604=CARTESIAN_POINT('',(5.1,3.1,2.));
#9605=CARTESIAN_POINT('Origin',(5.5,3.1,2.));
#9606=CARTESIAN_POINT('',(5.1,3.1,5.));
#9607=CARTESIAN_POINT('',(5.1,3.1,2.));
#9608=CARTESIAN_POINT('Origin',(5.5,3.1,5.));
#9609=CARTESIAN_POINT('Origin',(5.5,3.1,2.));
#9610=CARTESIAN_POINT('',(5.275,3.1,2.));
#9611=CARTESIAN_POINT('Origin',(5.5,3.1,2.));
#9612=CARTESIAN_POINT('Origin',(5.5,2.,5.));
#9613=CARTESIAN_POINT('',(5.,3.5,5.));
#9614=CARTESIAN_POINT('',(6.,0.5,5.));
#9615=CARTESIAN_POINT('Origin',(5.5,0.9,0.9));
#9616=CARTESIAN_POINT('',(5.275,0.9,1.));
#9617=CARTESIAN_POINT('Origin',(5.5,0.9,1.));
#9618=CARTESIAN_POINT('',(5.275,0.9,0.9));
#9619=CARTESIAN_POINT('Origin',(5.5,3.1,0.9));
#9620=CARTESIAN_POINT('',(5.275,3.1,1.));
#9621=CARTESIAN_POINT('Origin',(5.5,3.1,1.));
#9622=CARTESIAN_POINT('',(5.275,3.1,0.9));
#9623=CARTESIAN_POINT('Origin',(4.9,2.,4.));
#9624=CARTESIAN_POINT('',(5.,2.,4.6));
#9625=CARTESIAN_POINT('Origin',(5.,2.,4.));
#9626=CARTESIAN_POINT('',(4.9,2.,4.6));
#9627=CARTESIAN_POINT('',(6.,2.,4.6));
#9628=CARTESIAN_POINT('',(4.9,2.,4.6));
#9629=CARTESIAN_POINT('Origin',(6.,2.,4.));
#9630=CARTESIAN_POINT('Origin',(6.,0.5,1.));
#9631=CARTESIAN_POINT('',(6.,0.5,1.));
#9632=CARTESIAN_POINT('Origin',(5.,3.5,1.));
#9633=CARTESIAN_POINT('',(5.,3.5,1.));
#9634=CARTESIAN_POINT('Origin',(5.5,2.,1.));
#9635=CARTESIAN_POINT('',(0.,0.,0.));
#9636=CARTESIAN_POINT('Origin',(0.0577350269189626,0.,-0.1));
#9637=CARTESIAN_POINT('',(0.0577350269189626,0.,-0.1));
#9638=CARTESIAN_POINT('',(0.115470053837925,0.,0.));
#9639=CARTESIAN_POINT('',(0.0934187836487032,0.,-0.0381939203391614));
#9640=CARTESIAN_POINT('',(0.0577350269189626,-0.2,-0.1));
#9641=CARTESIAN_POINT('',(0.0577350269189626,0.,-0.1));
#9642=CARTESIAN_POINT('',(0.115470053837925,-0.2,0.));
#9643=CARTESIAN_POINT('',(0.115470053837925,-0.2,0.));
#9644=CARTESIAN_POINT('',(0.115470053837925,0.,0.));
#9645=CARTESIAN_POINT('Origin',(-0.0577350269189626,0.,-0.1));
#9646=CARTESIAN_POINT('',(-0.0577350269189626,0.,-0.1));
#9647=CARTESIAN_POINT('',(0.0561324865405187,0.,-0.1));
#9648=CARTESIAN_POINT('',(-0.0577350269189626,-0.2,-0.1));
#9649=CARTESIAN_POINT('',(-0.0577350269189626,0.,-0.1));
#9650=CARTESIAN_POINT('',(0.0577350269189626,-0.2,-0.1));
#9651=CARTESIAN_POINT('Origin',(-0.115470053837925,0.,-1.38777878078145E-17));
#9652=CARTESIAN_POINT('',(-0.115470053837925,0.,-1.41410031829988E-17));
#9653=CARTESIAN_POINT('',(-0.0797862971081845,0.,-0.0618060796608387));
#9654=CARTESIAN_POINT('',(-0.115470053837925,-0.2,-1.38777878078145E-17));
#9655=CARTESIAN_POINT('',(-0.115470053837925,0.,-1.41410031829988E-17));
#9656=CARTESIAN_POINT('',(-0.0577350269189626,-0.2,-0.1));
#9657=CARTESIAN_POINT('Origin',(-0.0577350269189626,0.,0.1));
#9658=CARTESIAN_POINT('',(-0.0577350269189626,0.,0.1));
#9659=CARTESIAN_POINT('',(-0.0509187836487033,0.,0.111806079660839));
#9660=CARTESIAN_POINT('',(-0.0577350269189626,-0.2,0.1));
#9661=CARTESIAN_POINT('',(-0.0577350269189626,0.,0.1));
#9662=CARTESIAN_POINT('',(-0.115470053837925,-0.2,-1.41410031829988E-17));
#9663=CARTESIAN_POINT('Origin',(0.0577350269189626,0.,0.1));
#9664=CARTESIAN_POINT('',(0.0577350269189626,0.,0.1));
#9665=CARTESIAN_POINT('',(0.113867513459481,0.,0.1));
#9666=CARTESIAN_POINT('',(0.0577350269189626,-0.2,0.1));
#9667=CARTESIAN_POINT('',(0.0577350269189626,0.,0.1));
#9668=CARTESIAN_POINT('',(-0.0577350269189626,-0.2,0.1));
#9669=CARTESIAN_POINT('Origin',(0.115470053837925,0.,0.));
#9670=CARTESIAN_POINT('',(0.122286297108185,0.,-0.0118060796608386));
#9671=CARTESIAN_POINT('',(0.0577350269189626,-0.2,0.1));
#9672=CARTESIAN_POINT('Origin',(0.,-0.2,0.));
#9673=CARTESIAN_POINT('Origin',(0.17,0.,0.));
#9674=CARTESIAN_POINT('',(-0.17,-8.67361737988404E-18,-2.0818995585505E-17));
#9675=CARTESIAN_POINT('Origin',(0.,0.,0.));
#9676=CARTESIAN_POINT('Origin',(0.,-0.015,0.));
#9677=CARTESIAN_POINT('',(-0.1954,-0.0254,-2.39295984553393E-17));
#9678=CARTESIAN_POINT('Origin',(0.,-0.0254,0.));
#9679=CARTESIAN_POINT('',(-0.185,-0.015,-2.2655965784226E-17));
#9680=CARTESIAN_POINT('Origin',(0.,-0.2775,0.));
#9681=CARTESIAN_POINT('',(-0.1954,-0.5296,2.39295984553393E-17));
#9682=CARTESIAN_POINT('Origin',(0.,-0.5296,0.));
#9683=CARTESIAN_POINT('',(-0.1954,-0.2775,-2.39295984553393E-17));
#9684=CARTESIAN_POINT('Origin',(0.,-0.5625,0.));
#9685=CARTESIAN_POINT('',(-0.125,-0.6,-1.53080849893419E-17));
#9686=CARTESIAN_POINT('Origin',(0.,-0.6,0.));
#9687=CARTESIAN_POINT('',(-0.1625,-0.5625,-1.99005104861445E-17));
#9688=CARTESIAN_POINT('Origin',(0.,-0.6,0.));
#9689=CARTESIAN_POINT('',(0.,0.,0.));
#9690=CARTESIAN_POINT('',(0.,0.,0.));
#9691=CARTESIAN_POINT('Origin',(4.,0.,4.7));
#9692=CARTESIAN_POINT('',(3.75,-3.06161699786838E-17,4.8));
#9693=CARTESIAN_POINT('Origin',(4.,0.,4.8));
#9694=CARTESIAN_POINT('',(3.75,3.06161699786838E-17,5.6));
#9695=CARTESIAN_POINT('',(3.75,-3.06161699786838E-17,4.7));
#9696=CARTESIAN_POINT('Origin',(4.,0.,5.6));
#9697=CARTESIAN_POINT('Origin',(0.,2.,4.7));
#9698=CARTESIAN_POINT('',(-0.25,2.,4.8));
#9699=CARTESIAN_POINT('Origin',(0.,2.,4.8));
#9700=CARTESIAN_POINT('',(-0.25,2.,5.6));
#9701=CARTESIAN_POINT('',(-0.25,2.,4.7));
#9702=CARTESIAN_POINT('Origin',(0.,2.,5.6));
#9703=CARTESIAN_POINT('Origin',(-2.5,-2.5,4.7));
#9704=CARTESIAN_POINT('',(-2.725,-2.5,4.8));
#9705=CARTESIAN_POINT('Origin',(-2.5,-2.5,4.8));
#9706=CARTESIAN_POINT('',(-2.725,-2.5,5.6));
#9707=CARTESIAN_POINT('',(-2.725,-2.5,4.7));
#9708=CARTESIAN_POINT('Origin',(-2.5,-2.5,5.6));
#9709=CARTESIAN_POINT('Origin',(-2.5,-2.5,4.8));
#9710=CARTESIAN_POINT('',(-2.41196534727688,-1.70485856609033,4.8));
#9711=CARTESIAN_POINT('',(-2.41196534727688,-1.70485856609033,5.6));
#9712=CARTESIAN_POINT('',(-2.41196534727688,-1.70485856609033,4.8));
#9713=CARTESIAN_POINT('',(-1.70485856609033,-2.41196534727688,4.8));
#9714=CARTESIAN_POINT('Origin',(-2.5,-2.5,4.8));
#9715=CARTESIAN_POINT('',(-1.70485856609033,-2.41196534727688,5.6));
#9716=CARTESIAN_POINT('',(-1.70485856609033,-2.41196534727688,4.8));
#9717=CARTESIAN_POINT('Origin',(-2.5,-2.5,5.6));
#9718=CARTESIAN_POINT('Origin',(-0.353553390593274,0.353553390593274,4.8));
#9719=CARTESIAN_POINT('',(-0.965925826289068,-0.25881904510252,5.6));
#9720=CARTESIAN_POINT('',(-2.85355339059327,-2.14644660940673,5.6));
#9721=CARTESIAN_POINT('',(-0.965925826289068,-0.258819045102521,4.8));
#9722=CARTESIAN_POINT('',(-0.965925826289068,-0.258819045102521,4.8));
#9723=CARTESIAN_POINT('',(-2.85355339059327,-2.14644660940673,4.8));
#9724=CARTESIAN_POINT('Origin',(0.,0.,5.6));
#9725=CARTESIAN_POINT('',(-0.258819045102521,-0.965925826289068,5.6));
#9726=CARTESIAN_POINT('',(0.353553390593274,-0.353553390593274,5.6));
#9727=CARTESIAN_POINT('',(0.866025403784439,-0.5,5.6));
#9728=CARTESIAN_POINT('Origin',(0.,0.,5.6));
#9729=CARTESIAN_POINT('',(3.37550020016016,-0.5,5.6));
#9730=CARTESIAN_POINT('',(4.,-0.5,5.6));
#9731=CARTESIAN_POINT('',(3.37550020016016,0.5,5.6));
#9732=CARTESIAN_POINT('Origin',(4.,0.,5.6));
#9733=CARTESIAN_POINT('',(0.866025403784439,0.5,5.6));
#9734=CARTESIAN_POINT('',(0.,0.5,5.6));
#9735=CARTESIAN_POINT('',(0.5,0.866025403784439,5.6));
#9736=CARTESIAN_POINT('Origin',(0.,0.,5.6));
#9737=CARTESIAN_POINT('',(0.5,1.37550020016016,5.6));
#9738=CARTESIAN_POINT('',(0.5,2.,5.6));
#9739=CARTESIAN_POINT('',(-0.5,1.37550020016016,5.6));
#9740=CARTESIAN_POINT('Origin',(0.,2.,5.6));
#9741=CARTESIAN_POINT('',(-0.5,0.866025403784439,5.6));
#9742=CARTESIAN_POINT('',(-0.5,0.,5.6));
#9743=CARTESIAN_POINT('Origin',(0.,0.,5.6));
#9744=CARTESIAN_POINT('Origin',(-2.14644660940673,-2.85355339059327,4.8));
#9745=CARTESIAN_POINT('',(-0.25881904510252,-0.965925826289068,4.8));
#9746=CARTESIAN_POINT('',(0.353553390593274,-0.353553390593274,4.8));
#9747=CARTESIAN_POINT('',(-0.25881904510252,-0.965925826289068,4.8));
#9748=CARTESIAN_POINT('Origin',(0.,0.,4.8));
#9749=CARTESIAN_POINT('',(-0.5,0.866025403784439,4.8));
#9750=CARTESIAN_POINT('',(-0.5,0.866025403784439,4.8));
#9751=CARTESIAN_POINT('Origin',(0.,0.,4.8));
#9752=CARTESIAN_POINT('Origin',(0.,0.,4.8));
#9753=CARTESIAN_POINT('',(0.866025403784439,-0.5,4.8));
#9754=CARTESIAN_POINT('Origin',(0.,0.,4.8));
#9755=CARTESIAN_POINT('',(0.866025403784439,-0.5,4.8));
#9756=CARTESIAN_POINT('Origin',(4.,0.,4.8));
#9757=CARTESIAN_POINT('',(3.37550020016016,0.5,4.8));
#9758=CARTESIAN_POINT('',(3.37550020016016,0.5,4.8));
#9759=CARTESIAN_POINT('',(3.37550020016016,-0.5,4.8));
#9760=CARTESIAN_POINT('',(3.37550020016016,-0.5,4.8));
#9761=CARTESIAN_POINT('Origin',(4.,0.,4.8));
#9762=CARTESIAN_POINT('Origin',(4.,0.5,4.8));
#9763=CARTESIAN_POINT('',(0.866025403784439,0.5,4.8));
#9764=CARTESIAN_POINT('',(0.,0.5,4.8));
#9765=CARTESIAN_POINT('',(0.866025403784439,0.5,4.8));
#9766=CARTESIAN_POINT('Origin',(0.,0.,4.8));
#9767=CARTESIAN_POINT('',(-0.5,1.37550020016016,4.8));
#9768=CARTESIAN_POINT('',(-0.5,0.,4.8));
#9769=CARTESIAN_POINT('',(0.5,1.37550020016016,4.8));
#9770=CARTESIAN_POINT('Origin',(0.,2.,4.8));
#9771=CARTESIAN_POINT('',(0.5,0.866025403784439,4.8));
#9772=CARTESIAN_POINT('',(0.5,2.,4.8));
#9773=CARTESIAN_POINT('Origin',(0.,0.,4.8));
#9774=CARTESIAN_POINT('',(4.,-0.5,4.8));
#9775=CARTESIAN_POINT('',(-0.7,-8.57252759403147E-17,4.8));
#9776=CARTESIAN_POINT('Origin',(0.,0.,4.8));
#9777=CARTESIAN_POINT('Origin',(0.,-0.5,4.8));
#9778=CARTESIAN_POINT('Origin',(0.,2.,4.8));
#9779=CARTESIAN_POINT('',(0.5,1.37550020016016,4.8));
#9780=CARTESIAN_POINT('',(-0.5,1.37550020016016,4.8));
#9781=CARTESIAN_POINT('Origin',(0.5,0.,4.8));
#9782=CARTESIAN_POINT('',(0.5,0.866025403784439,4.8));
#9783=CARTESIAN_POINT('Origin',(-0.5,2.,4.8));
#9784=CARTESIAN_POINT('Origin',(0.,0.,4.8));
#9785=CARTESIAN_POINT('Origin',(0.,0.,2.95));
#9786=CARTESIAN_POINT('',(-0.7,-8.57252759403147E-17,2.95));
#9787=CARTESIAN_POINT('Origin',(0.,0.,2.95));
#9788=CARTESIAN_POINT('',(-0.5,6.12323399573677E-17,2.95));
#9789=CARTESIAN_POINT('Origin',(0.,0.,2.95));
#9790=CARTESIAN_POINT('Origin',(0.,0.,2.95));
#9791=CARTESIAN_POINT('',(-0.7,-8.57252759403147E-17,2.95));
#9792=CARTESIAN_POINT('Origin',(0.,0.,1.));
#9793=CARTESIAN_POINT('',(-0.5,-6.12323399573677E-17,1.));
#9794=CARTESIAN_POINT('',(-0.5,-6.12323399573677E-17,1.));
#9795=CARTESIAN_POINT('Origin',(0.,0.,1.));
#9796=CARTESIAN_POINT('Origin',(0.,0.,1.));
#9797=CARTESIAN_POINT('',(0.,0.,0.));
#9798=CARTESIAN_POINT('Origin',(-2.5,-2.5,5.5));
#9799=CARTESIAN_POINT('',(-2.665,-2.5,5.6));
#9800=CARTESIAN_POINT('Origin',(-2.5,-2.5,5.6));
#9801=CARTESIAN_POINT('',(-2.665,-2.5,6.7));
#9802=CARTESIAN_POINT('',(-2.665,-2.5,5.5));
#9803=CARTESIAN_POINT('Origin',(-2.5,-2.5,6.7));
#9804=CARTESIAN_POINT('Origin',(-2.5,-2.5,6.7));
#9805=CARTESIAN_POINT('Origin',(-2.5,-2.5,5.6));
#9806=CARTESIAN_POINT('',(-3.1,-2.5,8.1));
#9807=CARTESIAN_POINT('Origin',(-2.5,-2.5,8.1));
#9808=CARTESIAN_POINT('',(-3.1,-2.5,5.6));
#9809=CARTESIAN_POINT('',(-3.1,-2.5,5.6));
#9810=CARTESIAN_POINT('Origin',(-2.5,-2.5,5.6));
#9811=CARTESIAN_POINT('Origin',(-2.5,-2.5,8.1));
#9812=CARTESIAN_POINT('Origin',(-2.5,-2.5,5.6));
#9813=CARTESIAN_POINT('',(0.,0.,0.));
#9814=CARTESIAN_POINT('Origin',(0.,0.,1.8));
#9815=CARTESIAN_POINT('',(-0.505,-6.18446633569413E-17,2.05));
#9816=CARTESIAN_POINT('Origin',(0.,0.,2.05));
#9817=CARTESIAN_POINT('',(-0.505,-6.18446633569413E-17,1.8));
#9818=CARTESIAN_POINT('',(-0.505,-6.18446633569413E-17,1.8));
#9819=CARTESIAN_POINT('Origin',(0.,0.,1.8));
#9820=CARTESIAN_POINT('Origin',(0.,0.,1.8));
#9821=CARTESIAN_POINT('',(-0.7,-8.57252759403147E-17,2.05));
#9822=CARTESIAN_POINT('Origin',(0.,0.,2.05));
#9823=CARTESIAN_POINT('',(-0.7,-8.57252759403147E-17,1.8));
#9824=CARTESIAN_POINT('',(-0.7,-8.57252759403147E-17,1.8));
#9825=CARTESIAN_POINT('Origin',(0.,0.,1.8));
#9826=CARTESIAN_POINT('Origin',(0.,0.,2.05));
#9827=CARTESIAN_POINT('Origin',(0.,0.,1.8));
#9828=CARTESIAN_POINT('',(0.,0.,0.));
#9829=CARTESIAN_POINT('Origin',(0.49,0.,1.4));
#9830=CARTESIAN_POINT('',(0.49,0.122167917228706,1.28909463493591));
#9831=CARTESIAN_POINT('',(0.49,0.122167917228706,1.51090536506409));
#9832=CARTESIAN_POINT('',(0.49,0.122167917228706,1.));
#9833=CARTESIAN_POINT('Origin',(0.49,0.,1.4));
#9834=CARTESIAN_POINT('Origin',(0.49,0.,1.4));
#9835=CARTESIAN_POINT('',(0.49,-0.122167917228706,1.28909463493591));
#9836=CARTESIAN_POINT('Ctrl Pts',(0.49,-0.122167917228706,1.28909463493591));
#9837=CARTESIAN_POINT('Ctrl Pts',(0.490448531679987,-0.120368913626296,
1.28711294069536));
#9838=CARTESIAN_POINT('Ctrl Pts',(0.490895245371685,-0.118534896565231,
1.28518965877367));
#9839=CARTESIAN_POINT('Ctrl Pts',(0.494795015531646,-0.102111993019358,
1.2687667552278));
#9840=CARTESIAN_POINT('Ctrl Pts',(0.498442514607594,-0.0836597150224318,
1.25609154388858));
#9841=CARTESIAN_POINT('Ctrl Pts',(0.50357781976106,-0.0430495960471595,
1.23920409039234));
#9842=CARTESIAN_POINT('Ctrl Pts',(0.505,-0.020880094330741,1.235));
#9843=CARTESIAN_POINT('Ctrl Pts',(0.505,0.020880094330741,1.235));
#9844=CARTESIAN_POINT('Ctrl Pts',(0.50357781976106,0.0430495960471595,1.23920409039234));
#9845=CARTESIAN_POINT('Ctrl Pts',(0.498442514607594,0.0836597150224318,
1.25609154388858));
#9846=CARTESIAN_POINT('Ctrl Pts',(0.494795015531646,0.102111993019358,1.2687667552278));
#9847=CARTESIAN_POINT('Ctrl Pts',(0.490895245371684,0.118534896565231,1.28518965877367));
#9848=CARTESIAN_POINT('Ctrl Pts',(0.490448531679987,0.120368913626296,1.28711294069536));
#9849=CARTESIAN_POINT('Ctrl Pts',(0.49,0.122167917228706,1.28909463493591));
#9850=CARTESIAN_POINT('',(0.49,-0.122167917228706,1.51090536506409));
#9851=CARTESIAN_POINT('Origin',(0.49,0.,1.4));
#9852=CARTESIAN_POINT('',(0.505,-1.70422299968729E-17,1.565));
#9853=CARTESIAN_POINT('Ctrl Pts',(0.505,-6.93889390390723E-18,1.565));
#9854=CARTESIAN_POINT('Ctrl Pts',(0.505,-0.020880094330741,1.565));
#9855=CARTESIAN_POINT('Ctrl Pts',(0.50357781976106,-0.0430495960471595,
1.56079590960766));
#9856=CARTESIAN_POINT('Ctrl Pts',(0.498442514607594,-0.0836597150224318,
1.54390845611142));
#9857=CARTESIAN_POINT('Ctrl Pts',(0.494795015531646,-0.102111993019358,
1.5312332447722));
#9858=CARTESIAN_POINT('Ctrl Pts',(0.490895245371684,-0.118534896565231,
1.51481034122633));
#9859=CARTESIAN_POINT('Ctrl Pts',(0.490448531679987,-0.120368913626296,
1.51288705930464));
#9860=CARTESIAN_POINT('Ctrl Pts',(0.49,-0.122167917228706,1.51090536506409));
#9861=CARTESIAN_POINT('',(0.9,-2.02066721859313E-17,1.565));
#9862=CARTESIAN_POINT('',(0.49,-2.02066721859313E-17,1.565));
#9863=CARTESIAN_POINT('',(0.884745726183518,0.165,1.4));
#9864=CARTESIAN_POINT('Ctrl Pts',(0.884745726183518,0.165,1.4));
#9865=CARTESIAN_POINT('Ctrl Pts',(0.884745726183518,0.165,1.37923124059256));
#9866=CARTESIAN_POINT('Ctrl Pts',(0.885552759505264,0.160839719007584,1.35711110492666));
#9867=CARTESIAN_POINT('Ctrl Pts',(0.888448648150043,0.143986470216691,1.31647293736623));
#9868=CARTESIAN_POINT('Ctrl Pts',(0.890493604851638,0.131295993814186,1.29795075602263));
#9869=CARTESIAN_POINT('Ctrl Pts',(0.89431723432394,0.102049819008125,1.26870458121656));
#9870=CARTESIAN_POINT('Ctrl Pts',(0.896347088899543,0.0835273920906824,
1.25601365401642));
#9871=CARTESIAN_POINT('Ctrl Pts',(0.899208271860583,0.0428883760934127,
1.23916007816136));
#9872=CARTESIAN_POINT('Ctrl Pts',(0.9,0.0207679427235068,1.235));
#9873=CARTESIAN_POINT('Ctrl Pts',(0.9,-0.0207679427235068,1.235));
#9874=CARTESIAN_POINT('Ctrl Pts',(0.899208271860583,-0.0428883760934127,
1.23916007816136));
#9875=CARTESIAN_POINT('Ctrl Pts',(0.896347088899543,-0.0835273920906823,
1.25601365401642));
#9876=CARTESIAN_POINT('Ctrl Pts',(0.89431723432394,-0.102049819008125,1.26870458121656));
#9877=CARTESIAN_POINT('Ctrl Pts',(0.890493604851638,-0.131295993814186,
1.29795075602263));
#9878=CARTESIAN_POINT('Ctrl Pts',(0.888448648150043,-0.143986470216691,
1.31647293736623));
#9879=CARTESIAN_POINT('Ctrl Pts',(0.885552759505264,-0.160839719007584,
1.35711110492666));
#9880=CARTESIAN_POINT('Ctrl Pts',(0.884745726183518,-0.165,1.37923124059256));
#9881=CARTESIAN_POINT('Ctrl Pts',(0.884745726183518,-0.165,1.42076875940744));
#9882=CARTESIAN_POINT('Ctrl Pts',(0.885552759505264,-0.160839719007584,
1.44288889507334));
#9883=CARTESIAN_POINT('Ctrl Pts',(0.888448648150043,-0.14398647021669,1.48352706263377));
#9884=CARTESIAN_POINT('Ctrl Pts',(0.890493604851638,-0.131295993814186,
1.50204924397737));
#9885=CARTESIAN_POINT('Ctrl Pts',(0.89431723432394,-0.102049819008125,1.53129541878344));
#9886=CARTESIAN_POINT('Ctrl Pts',(0.896347088899543,-0.0835273920906824,
1.54398634598358));
#9887=CARTESIAN_POINT('Ctrl Pts',(0.899208271860583,-0.0428883760934128,
1.56083992183864));
#9888=CARTESIAN_POINT('Ctrl Pts',(0.9,-0.0207679427235068,1.565));
#9889=CARTESIAN_POINT('Ctrl Pts',(0.9,-6.93889390390723E-18,1.565));
#9890=CARTESIAN_POINT('Ctrl Pts',(0.9,-3.46944695195361E-17,1.565));
#9891=CARTESIAN_POINT('Ctrl Pts',(0.9,0.0207679427235068,1.565));
#9892=CARTESIAN_POINT('Ctrl Pts',(0.899208271860583,0.0428883760934127,
1.56083992183864));
#9893=CARTESIAN_POINT('Ctrl Pts',(0.896347088899543,0.0835273920906824,
1.54398634598358));
#9894=CARTESIAN_POINT('Ctrl Pts',(0.89431723432394,0.102049819008125,1.53129541878344));
#9895=CARTESIAN_POINT('Ctrl Pts',(0.890493604851638,0.131295993814186,1.50204924397737));
#9896=CARTESIAN_POINT('Ctrl Pts',(0.888448648150043,0.143986470216691,1.48352706263377));
#9897=CARTESIAN_POINT('Ctrl Pts',(0.885552759505264,0.160839719007584,1.44288889507334));
#9898=CARTESIAN_POINT('Ctrl Pts',(0.884745726183518,0.165,1.42076875940744));
#9899=CARTESIAN_POINT('Ctrl Pts',(0.884745726183518,0.165,1.4));
#9900=CARTESIAN_POINT('Ctrl Pts',(0.49,0.122167917228706,1.51090536506409));
#9901=CARTESIAN_POINT('Ctrl Pts',(0.490448531679987,0.120368913626296,1.51288705930464));
#9902=CARTESIAN_POINT('Ctrl Pts',(0.490895245371685,0.118534896565231,1.51481034122633));
#9903=CARTESIAN_POINT('Ctrl Pts',(0.494795015531646,0.102111993019358,1.5312332447722));
#9904=CARTESIAN_POINT('Ctrl Pts',(0.498442514607594,0.0836597150224318,
1.54390845611142));
#9905=CARTESIAN_POINT('Ctrl Pts',(0.50357781976106,0.0430495960471594,1.56079590960766));
#9906=CARTESIAN_POINT('Ctrl Pts',(0.505,0.020880094330741,1.565));
#9907=CARTESIAN_POINT('Ctrl Pts',(0.505,0.,1.565));
#9908=CARTESIAN_POINT('Origin',(0.49,0.,1.4));
#9909=CARTESIAN_POINT('',(0.49,-0.122167917228706,1.));
#9910=CARTESIAN_POINT('Origin',(0.,0.,1.));
#9911=CARTESIAN_POINT('',(-0.505,-6.18446633569413E-17,1.8));
#9912=CARTESIAN_POINT('Origin',(0.,0.,1.8));
#9913=CARTESIAN_POINT('',(-0.505,-6.18446633569413E-17,1.));
#9914=CARTESIAN_POINT('',(-0.505,-6.18446633569413E-17,1.));
#9915=CARTESIAN_POINT('Origin',(0.,0.,1.));
#9916=CARTESIAN_POINT('Origin',(0.,0.,1.));
#9917=CARTESIAN_POINT('',(-0.9,-1.10218211923262E-16,1.8));
#9918=CARTESIAN_POINT('Origin',(0.,0.,1.8));
#9919=CARTESIAN_POINT('',(-0.9,-1.10218211923262E-16,1.));
#9920=CARTESIAN_POINT('',(-0.9,-1.10218211923262E-16,1.));
#9921=CARTESIAN_POINT('Origin',(0.,0.,1.));
#9922=CARTESIAN_POINT('Origin',(0.,0.,1.8));
#9923=CARTESIAN_POINT('Origin',(0.,0.,1.));
#9924=CARTESIAN_POINT('',(0.,0.,0.));
#9925=CARTESIAN_POINT('Origin',(0.3,0.4,0.));
#9926=CARTESIAN_POINT('',(-0.3,0.4,-3.67394039744206E-17));
#9927=CARTESIAN_POINT('Origin',(0.,0.4,0.));
#9928=CARTESIAN_POINT('Origin',(0.,0.375,0.));
#9929=CARTESIAN_POINT('',(-0.35,0.35,-4.28626379701573E-17));
#9930=CARTESIAN_POINT('Origin',(0.,0.35,0.));
#9931=CARTESIAN_POINT('',(-0.325,0.375,-3.9801020972289E-17));
#9932=CARTESIAN_POINT('Origin',(0.,0.19,0.));
#9933=CARTESIAN_POINT('',(-0.35,0.03,-4.28626379701574E-17));
#9934=CARTESIAN_POINT('Origin',(0.,0.03,0.));
#9935=CARTESIAN_POINT('',(-0.35,0.19,-4.28626379701574E-17));
#9936=CARTESIAN_POINT('Origin',(0.,0.0149999999999999,0.));
#9937=CARTESIAN_POINT('',(-0.32,-3.29597460435593E-17,-3.91886975727153E-17));
#9938=CARTESIAN_POINT('Origin',(0.,0.,0.));
#9939=CARTESIAN_POINT('',(-0.335,0.0149999999999999,-4.10256677714363E-17));
#9940=CARTESIAN_POINT('Origin',(0.22,0.,0.));
#9941=CARTESIAN_POINT('',(-0.22,-6.93889390390723E-18,-2.69422295812418E-17));
#9942=CARTESIAN_POINT('Origin',(0.,0.,0.));
#9943=CARTESIAN_POINT('Origin',(0.,-0.02,0.));
#9944=CARTESIAN_POINT('',(-0.1954,-0.0492,2.39295984553393E-17));
#9945=CARTESIAN_POINT('Origin',(0.,-0.0492,0.));
#9946=CARTESIAN_POINT('',(-0.21,-0.02,-2.57175827820944E-17));
#9947=CARTESIAN_POINT('Origin',(0.,-0.8,0.));
#9948=CARTESIAN_POINT('',(-0.1954,-1.5646,2.39295984553393E-17));
#9949=CARTESIAN_POINT('Origin',(0.,-1.5646,0.));
#9950=CARTESIAN_POINT('',(-0.1954,-0.8,-2.39295984553393E-17));
#9951=CARTESIAN_POINT('Origin',(0.,-1.58,0.));
#9952=CARTESIAN_POINT('',(-0.16,-1.6,-1.95943487863577E-17));
#9953=CARTESIAN_POINT('Origin',(0.,-1.6,0.));
#9954=CARTESIAN_POINT('',(-0.18,-1.58,-2.20436423846524E-17));
#9955=CARTESIAN_POINT('Origin',(0.,-1.6,0.));
#9956=CARTESIAN_POINT('Origin',(0.0866025403784439,-0.4,-0.15));
#9957=CARTESIAN_POINT('',(0.173205080756888,-0.4,0.));
#9958=CARTESIAN_POINT('',(0.0866025403784439,-0.4,-0.15));
#9959=CARTESIAN_POINT('',(0.173205080756888,-0.4,0.));
#9960=CARTESIAN_POINT('',(0.0866025403784439,-0.64,-0.15));
#9961=CARTESIAN_POINT('',(0.0866025403784439,-0.4,-0.15));
#9962=CARTESIAN_POINT('',(0.173205080756888,-0.64,0.));
#9963=CARTESIAN_POINT('',(0.173205080756888,-0.64,0.));
#9964=CARTESIAN_POINT('',(0.173205080756888,-0.4,0.));
#9965=CARTESIAN_POINT('Origin',(-0.0866025403784438,-0.4,-0.15));
#9966=CARTESIAN_POINT('',(-0.0866025403784438,-0.4,-0.15));
#9967=CARTESIAN_POINT('',(0.0866025403784439,-0.4,-0.15));
#9968=CARTESIAN_POINT('',(-0.0866025403784438,-0.64,-0.15));
#9969=CARTESIAN_POINT('',(-0.0866025403784438,-0.4,-0.15));
#9970=CARTESIAN_POINT('',(0.0866025403784439,-0.64,-0.15));
#9971=CARTESIAN_POINT('Origin',(-0.173205080756888,-0.4,-2.77555756156289E-17));
#9972=CARTESIAN_POINT('',(-0.173205080756888,-0.4,-2.12115047744981E-17));
#9973=CARTESIAN_POINT('',(-0.0866025403784438,-0.4,-0.15));
#9974=CARTESIAN_POINT('',(-0.173205080756888,-0.64,-2.77555756156289E-17));
#9975=CARTESIAN_POINT('',(-0.173205080756888,-0.4,-2.12115047744981E-17));
#9976=CARTESIAN_POINT('',(-0.0866025403784438,-0.64,-0.15));
#9977=CARTESIAN_POINT('Origin',(-0.0866025403784439,-0.4,0.15));
#9978=CARTESIAN_POINT('',(-0.0866025403784439,-0.4,0.15));
#9979=CARTESIAN_POINT('',(-0.173205080756888,-0.4,-2.12115047744981E-17));
#9980=CARTESIAN_POINT('',(-0.0866025403784439,-0.64,0.15));
#9981=CARTESIAN_POINT('',(-0.0866025403784439,-0.4,0.15));
#9982=CARTESIAN_POINT('',(-0.173205080756888,-0.64,-2.12115047744981E-17));
#9983=CARTESIAN_POINT('Origin',(0.0866025403784439,-0.4,0.15));
#9984=CARTESIAN_POINT('',(0.0866025403784439,-0.4,0.15));
#9985=CARTESIAN_POINT('',(-0.0866025403784439,-0.4,0.15));
#9986=CARTESIAN_POINT('',(0.0866025403784439,-0.64,0.15));
#9987=CARTESIAN_POINT('',(0.0866025403784439,-0.4,0.15));
#9988=CARTESIAN_POINT('',(-0.0866025403784439,-0.64,0.15));
#9989=CARTESIAN_POINT('Origin',(0.173205080756888,-0.4,0.));
#9990=CARTESIAN_POINT('',(0.0866025403784439,-0.4,0.15));
#9991=CARTESIAN_POINT('',(0.0866025403784439,-0.64,0.15));
#9992=CARTESIAN_POINT('Origin',(0.,-0.4,-2.77555756156289E-17));
#9993=CARTESIAN_POINT('Origin',(0.,-0.64,-2.77555756156289E-17));
#9994=CARTESIAN_POINT('',(0.,0.,0.));
#9995=CARTESIAN_POINT('Origin',(0.,-0.4,0.));
#9996=CARTESIAN_POINT('',(-0.1954,-0.4,2.39295984553393E-17));
#9997=CARTESIAN_POINT('Origin',(0.,-0.4,0.));
#9998=CARTESIAN_POINT('Origin',(0.0577350269189626,0.,-0.1));
#9999=CARTESIAN_POINT('',(0.0577350269189626,0.,-0.1));
#10000=CARTESIAN_POINT('',(0.115470053837925,0.,0.));
#10001=CARTESIAN_POINT('',(0.0934187836487032,0.,-0.0381939203391614));
#10002=CARTESIAN_POINT('',(0.0577350269189626,-0.2,-0.1));
#10003=CARTESIAN_POINT('',(0.0577350269189626,0.,-0.1));
#10004=CARTESIAN_POINT('',(0.115470053837925,-0.2,0.));
#10005=CARTESIAN_POINT('',(0.115470053837925,-0.2,0.));
#10006=CARTESIAN_POINT('',(0.115470053837925,0.,0.));
#10007=CARTESIAN_POINT('Origin',(-0.0577350269189626,0.,-0.1));
#10008=CARTESIAN_POINT('',(-0.0577350269189626,0.,-0.1));
#10009=CARTESIAN_POINT('',(0.0561324865405187,0.,-0.1));
#10010=CARTESIAN_POINT('',(-0.0577350269189626,-0.2,-0.1));
#10011=CARTESIAN_POINT('',(-0.0577350269189626,0.,-0.1));
#10012=CARTESIAN_POINT('',(0.0577350269189626,-0.2,-0.1));
#10013=CARTESIAN_POINT('Origin',(-0.115470053837925,0.,-1.38777878078145E-17));
#10014=CARTESIAN_POINT('',(-0.115470053837925,0.,-1.41410031829988E-17));
#10015=CARTESIAN_POINT('',(-0.0797862971081845,0.,-0.0618060796608387));
#10016=CARTESIAN_POINT('',(-0.115470053837925,-0.2,-1.38777878078145E-17));
#10017=CARTESIAN_POINT('',(-0.115470053837925,0.,-1.41410031829988E-17));
#10018=CARTESIAN_POINT('',(-0.0577350269189626,-0.2,-0.1));
#10019=CARTESIAN_POINT('Origin',(-0.0577350269189626,0.,0.1));
#10020=CARTESIAN_POINT('',(-0.0577350269189626,0.,0.1));
#10021=CARTESIAN_POINT('',(-0.0509187836487033,0.,0.111806079660839));
#10022=CARTESIAN_POINT('',(-0.0577350269189626,-0.2,0.1));
#10023=CARTESIAN_POINT('',(-0.0577350269189626,0.,0.1));
#10024=CARTESIAN_POINT('',(-0.115470053837925,-0.2,-1.41410031829988E-17));
#10025=CARTESIAN_POINT('Origin',(0.0577350269189626,0.,0.1));
#10026=CARTESIAN_POINT('',(0.0577350269189626,0.,0.1));
#10027=CARTESIAN_POINT('',(0.113867513459481,0.,0.1));
#10028=CARTESIAN_POINT('',(0.0577350269189626,-0.2,0.1));
#10029=CARTESIAN_POINT('',(0.0577350269189626,0.,0.1));
#10030=CARTESIAN_POINT('',(-0.0577350269189626,-0.2,0.1));
#10031=CARTESIAN_POINT('Origin',(0.115470053837925,0.,0.));
#10032=CARTESIAN_POINT('',(0.122286297108185,0.,-0.0118060796608386));
#10033=CARTESIAN_POINT('',(0.0577350269189626,-0.2,0.1));
#10034=CARTESIAN_POINT('Origin',(0.,-0.2,0.));
#10035=CARTESIAN_POINT('Origin',(0.17,0.,0.));
#10036=CARTESIAN_POINT('',(-0.17,-8.67361737988404E-18,-2.0818995585505E-17));
#10037=CARTESIAN_POINT('Origin',(0.,0.,0.));
#10038=CARTESIAN_POINT('Origin',(0.,-0.015,0.));
#10039=CARTESIAN_POINT('',(-0.1954,-0.0254,-2.39295984553393E-17));
#10040=CARTESIAN_POINT('Origin',(0.,-0.0254,0.));
#10041=CARTESIAN_POINT('',(-0.185,-0.015,-2.2655965784226E-17));
#10042=CARTESIAN_POINT('Origin',(0.,-0.2775,0.));
#10043=CARTESIAN_POINT('',(-0.1954,-0.2775,-2.39295984553393E-17));
#10044=CARTESIAN_POINT('',(0.,0.,0.));
#10045=CARTESIAN_POINT('Origin',(0.,2.,9.1));
#10046=CARTESIAN_POINT('',(-0.165,2.,9.1));
#10047=CARTESIAN_POINT('Origin',(0.,2.,9.1));
#10048=CARTESIAN_POINT('',(-0.165,2.,10.1));
#10049=CARTESIAN_POINT('',(-0.165,2.,9.1));
#10050=CARTESIAN_POINT('Origin',(0.,2.,10.1));
#10051=CARTESIAN_POINT('Origin',(0.,2.,9.1));
#10052=CARTESIAN_POINT('Origin',(0.,2.,6.));
#10053=CARTESIAN_POINT('',(-0.7,2.,6.));
#10054=CARTESIAN_POINT('Origin',(0.,2.,6.));
#10055=CARTESIAN_POINT('',(-0.3,2.,6.));
#10056=CARTESIAN_POINT('Origin',(0.,2.,6.));
#10057=CARTESIAN_POINT('Origin',(0.,2.,5.6));
#10058=CARTESIAN_POINT('',(-0.7,2.,5.6));
#10059=CARTESIAN_POINT('Origin',(0.,2.,5.6));
#10060=CARTESIAN_POINT('',(-0.3,2.,5.6));
#10061=CARTESIAN_POINT('Origin',(0.,2.,5.6));
#10062=CARTESIAN_POINT('Origin',(0.,2.,5.6));
#10063=CARTESIAN_POINT('',(-0.7,2.,5.6));
#10064=CARTESIAN_POINT('Origin',(0.,2.,4.8));
#10065=CARTESIAN_POINT('',(-0.3,2.,4.8));
#10066=CARTESIAN_POINT('',(-0.3,2.,4.8));
#10067=CARTESIAN_POINT('Origin',(0.,2.,4.8));
#10068=CARTESIAN_POINT('Origin',(0.,2.,4.8));
#10069=CARTESIAN_POINT('',(-0.3,2.,10.1));
#10070=CARTESIAN_POINT('Origin',(0.,2.,10.1));
#10071=CARTESIAN_POINT('',(-0.3,2.,4.8));
#10072=CARTESIAN_POINT('Origin',(0.,2.,10.1));
#10073=CARTESIAN_POINT('Origin',(0.,2.,4.8));
#10074=CARTESIAN_POINT('',(0.,0.,0.));
#10075=CARTESIAN_POINT('Origin',(0.,2.,6.));
#10076=CARTESIAN_POINT('',(-0.305,2.,8.8));
#10077=CARTESIAN_POINT('Origin',(0.,2.,8.8));
#10078=CARTESIAN_POINT('',(-0.305,2.,6.));
#10079=CARTESIAN_POINT('',(-0.305,2.,6.));
#10080=CARTESIAN_POINT('Origin',(0.,2.,6.));
#10081=CARTESIAN_POINT('Origin',(0.,2.,6.));
#10082=CARTESIAN_POINT('',(-0.5,2.,8.8));
#10083=CARTESIAN_POINT('Origin',(0.,2.,8.8));
#10084=CARTESIAN_POINT('',(-0.5,2.,6.));
#10085=CARTESIAN_POINT('',(-0.5,2.,6.));
#10086=CARTESIAN_POINT('Origin',(0.,2.,6.));
#10087=CARTESIAN_POINT('Origin',(0.,2.,8.8));
#10088=CARTESIAN_POINT('Origin',(0.,2.,6.));
#10089=CARTESIAN_POINT('',(0.,0.,0.));
#10090=CARTESIAN_POINT('',(0.,0.,0.));
#10091=CARTESIAN_POINT('Origin',(0.,2.,8.7));
#10092=CARTESIAN_POINT('',(-0.5,2.,8.8));
#10093=CARTESIAN_POINT('Origin',(0.,2.,8.8));
#10094=CARTESIAN_POINT('',(-0.5,2.,9.6));
#10095=CARTESIAN_POINT('',(-0.5,2.,8.7));
#10096=CARTESIAN_POINT('Origin',(0.,2.,9.6));
#10097=CARTESIAN_POINT('Origin',(7.5,4.,8.7));
#10098=CARTESIAN_POINT('',(7.,4.,8.8));
#10099=CARTESIAN_POINT('Origin',(7.5,4.,8.8));
#10100=CARTESIAN_POINT('',(7.,4.,9.6));
#10101=CARTESIAN_POINT('',(7.,4.,8.7));
#10102=CARTESIAN_POINT('Origin',(7.5,4.,9.6));
#10103=CARTESIAN_POINT('Origin',(7.5,4.,8.8));
#10104=CARTESIAN_POINT('',(6.7677551483406,4.32220719609949,9.6));
#10105=CARTESIAN_POINT('',(6.7677551483406,4.32220719609949,8.8));
#10106=CARTESIAN_POINT('',(6.7677551483406,4.32220719609949,8.8));
#10107=CARTESIAN_POINT('',(7.02541779890093,3.35597225649825,9.6));
#10108=CARTESIAN_POINT('Origin',(7.5,4.,9.6));
#10109=CARTESIAN_POINT('',(7.02541779890093,3.35597225649825,8.8));
#10110=CARTESIAN_POINT('',(7.02541779890093,3.35597225649825,8.8));
#10111=CARTESIAN_POINT('Origin',(7.5,4.,8.8));
#10112=CARTESIAN_POINT('Origin',(7.37116867471983,4.48311746980062,8.8));
#10113=CARTESIAN_POINT('',(0.474582201099072,2.64402774350175,8.8));
#10114=CARTESIAN_POINT('',(-0.128831325280166,2.48311746980062,8.8));
#10115=CARTESIAN_POINT('',(0.474582201099072,2.64402774350175,9.6));
#10116=CARTESIAN_POINT('',(0.474582201099072,2.64402774350175,8.8));
#10117=CARTESIAN_POINT('',(-0.128831325280166,2.48311746980062,9.6));
#10118=CARTESIAN_POINT('Origin',(0.,2.,8.8));
#10119=CARTESIAN_POINT('',(0.732244851659405,1.67779280390051,8.8));
#10120=CARTESIAN_POINT('',(7.62883132528017,3.51688253019938,8.8));
#10121=CARTESIAN_POINT('Origin',(0.,2.,8.8));
#10122=CARTESIAN_POINT('Origin',(0.128831325280166,1.51688253019938,8.8));
#10123=CARTESIAN_POINT('',(0.732244851659405,1.67779280390051,9.6));
#10124=CARTESIAN_POINT('',(7.62883132528017,3.51688253019938,9.6));
#10125=CARTESIAN_POINT('',(0.732244851659405,1.67779280390051,8.8));
#10126=CARTESIAN_POINT('Origin',(0.,2.,8.8));
#10127=CARTESIAN_POINT('Origin',(0.,2.,9.6));
#10128=CARTESIAN_POINT('Origin',(0.,2.,9.6));
#10129=CARTESIAN_POINT('',(0.,0.,0.));
#10130=CARTESIAN_POINT('Origin',(0.,2.,8.8));
#10131=CARTESIAN_POINT('',(-0.305,2.,9.6));
#10132=CARTESIAN_POINT('Origin',(0.,2.,9.6));
#10133=CARTESIAN_POINT('',(-0.305,2.,8.8));
#10134=CARTESIAN_POINT('',(-0.305,2.,8.8));
#10135=CARTESIAN_POINT('Origin',(0.,2.,8.8));
#10136=CARTESIAN_POINT('Origin',(0.,2.,8.8));
#10137=CARTESIAN_POINT('',(-0.5,2.,9.6));
#10138=CARTESIAN_POINT('Origin',(0.,2.,9.6));
#10139=CARTESIAN_POINT('',(-0.5,2.,8.8));
#10140=CARTESIAN_POINT('',(-0.5,2.,8.8));
#10141=CARTESIAN_POINT('Origin',(0.,2.,8.8));
#10142=CARTESIAN_POINT('Origin',(0.,2.,9.6));
#10143=CARTESIAN_POINT('Origin',(0.,2.,8.8));
#10144=CARTESIAN_POINT('',(0.,0.,0.));
#10145=CARTESIAN_POINT('',(0.,0.,0.));
#10146=CARTESIAN_POINT('',(7.5,2.,0.));
#10147=CARTESIAN_POINT('',(0.,0.,0.));
#10148=CARTESIAN_POINT('',(0.,0.,0.));
#10149=CARTESIAN_POINT('Origin',(7.5,4.,9.1));
#10150=CARTESIAN_POINT('',(7.335,4.,9.1));
#10151=CARTESIAN_POINT('Origin',(7.5,4.,9.1));
#10152=CARTESIAN_POINT('',(7.335,4.,10.1));
#10153=CARTESIAN_POINT('',(7.335,4.,9.1));
#10154=CARTESIAN_POINT('Origin',(7.5,4.,10.1));
#10155=CARTESIAN_POINT('Origin',(7.5,4.,9.1));
#10156=CARTESIAN_POINT('Origin',(7.5,4.,6.1));
#10157=CARTESIAN_POINT('',(6.8,4.,6.1));
#10158=CARTESIAN_POINT('Origin',(7.5,4.,6.1));
#10159=CARTESIAN_POINT('',(7.2,4.,6.1));
#10160=CARTESIAN_POINT('Origin',(7.5,4.,6.1));
#10161=CARTESIAN_POINT('Origin',(7.5,4.,5.7));
#10162=CARTESIAN_POINT('',(6.8,4.,5.7));
#10163=CARTESIAN_POINT('Origin',(7.5,4.,5.7));
#10164=CARTESIAN_POINT('',(7.2,4.,5.7));
#10165=CARTESIAN_POINT('Origin',(7.5,4.,5.7));
#10166=CARTESIAN_POINT('Origin',(7.5,4.,5.7));
#10167=CARTESIAN_POINT('',(6.8,4.,5.7));
#10168=CARTESIAN_POINT('Origin',(7.5,4.,5.2));
#10169=CARTESIAN_POINT('',(7.2,4.,5.2));
#10170=CARTESIAN_POINT('',(7.2,4.,5.2));
#10171=CARTESIAN_POINT('Origin',(7.5,4.,5.2));
#10172=CARTESIAN_POINT('Origin',(7.5,4.,5.2));
#10173=CARTESIAN_POINT('',(7.2,4.,10.1));
#10174=CARTESIAN_POINT('Origin',(7.5,4.,10.1));
#10175=CARTESIAN_POINT('',(7.2,4.,5.2));
#10176=CARTESIAN_POINT('Origin',(7.5,4.,10.1));
#10177=CARTESIAN_POINT('Origin',(7.5,4.,5.2));
#10178=CARTESIAN_POINT('',(0.,0.,0.));
#10179=CARTESIAN_POINT('Origin',(7.5,4.,6.1));
#10180=CARTESIAN_POINT('',(7.195,4.,8.8));
#10181=CARTESIAN_POINT('Origin',(7.5,4.,8.8));
#10182=CARTESIAN_POINT('',(7.195,4.,6.1));
#10183=CARTESIAN_POINT('',(7.195,4.,6.1));
#10184=CARTESIAN_POINT('Origin',(7.5,4.,6.1));
#10185=CARTESIAN_POINT('Origin',(7.5,4.,6.1));
#10186=CARTESIAN_POINT('',(7.,4.,8.8));
#10187=CARTESIAN_POINT('Origin',(7.5,4.,8.8));
#10188=CARTESIAN_POINT('',(7.,4.,6.1));
#10189=CARTESIAN_POINT('',(7.,4.,6.1));
#10190=CARTESIAN_POINT('Origin',(7.5,4.,6.1));
#10191=CARTESIAN_POINT('Origin',(7.5,4.,8.8));
#10192=CARTESIAN_POINT('Origin',(7.5,4.,6.1));
#10193=CARTESIAN_POINT('',(0.,0.,0.));
#10194=CARTESIAN_POINT('Origin',(10.,2.,5.19));
#10195=CARTESIAN_POINT('',(9.75,2.,5.19));
#10196=CARTESIAN_POINT('Origin',(10.,2.,5.19));
#10197=CARTESIAN_POINT('',(9.75,2.,5.7));
#10198=CARTESIAN_POINT('',(9.75,2.,5.19));
#10199=CARTESIAN_POINT('Origin',(10.,2.,5.7));
#10200=CARTESIAN_POINT('Origin',(10.,2.,5.19));
#10201=CARTESIAN_POINT('Origin',(8.4,3.2,2.8));
#10202=CARTESIAN_POINT('',(8.5,3.2,2.965));
#10203=CARTESIAN_POINT('Origin',(8.5,3.2,2.8));
#10204=CARTESIAN_POINT('',(11.5,3.2,2.965));
#10205=CARTESIAN_POINT('',(8.4,3.2,2.965));
#10206=CARTESIAN_POINT('Origin',(11.5,3.2,2.8));
#10207=CARTESIAN_POINT('Origin',(8.4,0.8,5.2));
#10208=CARTESIAN_POINT('',(8.5,0.8,5.365));
#10209=CARTESIAN_POINT('Origin',(8.5,0.8,5.2));
#10210=CARTESIAN_POINT('',(11.5,0.8,5.365));
#10211=CARTESIAN_POINT('',(8.4,0.8,5.365));
#10212=CARTESIAN_POINT('Origin',(11.5,0.8,5.2));
#10213=CARTESIAN_POINT('Origin',(8.4,0.8,2.8));
#10214=CARTESIAN_POINT('',(8.5,0.8,2.965));
#10215=CARTESIAN_POINT('Origin',(8.5,0.8,2.8));
#10216=CARTESIAN_POINT('',(11.5,0.8,2.965));
#10217=CARTESIAN_POINT('',(8.4,0.8,2.965));
#10218=CARTESIAN_POINT('Origin',(11.5,0.8,2.8));
#10219=CARTESIAN_POINT('Origin',(8.4,3.2,5.2));
#10220=CARTESIAN_POINT('',(8.5,3.2,5.365));
#10221=CARTESIAN_POINT('Origin',(8.5,3.2,5.2));
#10222=CARTESIAN_POINT('',(11.5,3.2,5.365));
#10223=CARTESIAN_POINT('',(8.4,3.2,5.365));
#10224=CARTESIAN_POINT('Origin',(11.5,3.2,5.2));
#10225=CARTESIAN_POINT('Origin',(8.4,2.,4.));
#10226=CARTESIAN_POINT('',(8.5,2.,5.05));
#10227=CARTESIAN_POINT('Origin',(8.5,2.,4.));
#10228=CARTESIAN_POINT('',(11.5,2.,5.05));
#10229=CARTESIAN_POINT('',(8.4,2.,5.05));
#10230=CARTESIAN_POINT('Origin',(11.5,2.,4.));
#10231=CARTESIAN_POINT('Origin',(11.5,3.7,2.3));
#10232=CARTESIAN_POINT('',(11.5,3.7,2.3));
#10233=CARTESIAN_POINT('',(8.5,3.7,2.3));
#10234=CARTESIAN_POINT('',(11.5,3.7,2.3));
#10235=CARTESIAN_POINT('',(8.5,3.7,5.7));
#10236=CARTESIAN_POINT('',(8.5,3.7,2.3));
#10237=CARTESIAN_POINT('',(11.5,3.7,5.7));
#10238=CARTESIAN_POINT('',(11.5,3.7,5.7));
#10239=CARTESIAN_POINT('',(11.5,3.7,2.3));
#10240=CARTESIAN_POINT('Origin',(11.5,0.3,2.3));
#10241=CARTESIAN_POINT('',(11.5,0.3,2.3));
#10242=CARTESIAN_POINT('',(11.5,0.3,2.3));
#10243=CARTESIAN_POINT('',(11.5,0.3,5.7));
#10244=CARTESIAN_POINT('',(11.5,0.3,5.7));
#10245=CARTESIAN_POINT('',(11.5,0.3,2.3));
#10246=CARTESIAN_POINT('Origin',(8.5,0.3,2.3));
#10247=CARTESIAN_POINT('',(8.5,0.3,2.3));
#10248=CARTESIAN_POINT('',(8.5,0.3,2.3));
#10249=CARTESIAN_POINT('',(8.5,0.3,5.7));
#10250=CARTESIAN_POINT('',(8.5,0.3,5.7));
#10251=CARTESIAN_POINT('',(8.5,0.3,2.3));
#10252=CARTESIAN_POINT('Origin',(8.5,3.7,2.3));
#10253=CARTESIAN_POINT('',(8.5,3.7,2.3));
#10254=CARTESIAN_POINT('',(8.5,3.7,5.7));
#10255=CARTESIAN_POINT('Origin',(10.,2.,5.7));
#10256=CARTESIAN_POINT('Origin',(10.,2.,2.3));
#10257=CARTESIAN_POINT('',(0.,0.,0.));
#10258=CARTESIAN_POINT('',(0.,0.,0.));
#10259=CARTESIAN_POINT('Origin',(0.75,1.2,0.));
#10260=CARTESIAN_POINT('',(0.885663593019381,1.2,-0.16));
#10261=CARTESIAN_POINT('',(0.885663593019381,1.2,0.16));
#10262=CARTESIAN_POINT('Origin',(0.,1.2,0.));
#10263=CARTESIAN_POINT('',(0.93,1.2,-0.16));
#10264=CARTESIAN_POINT('',(0.93,1.2,-0.16));
#10265=CARTESIAN_POINT('',(0.93,1.2,0.16));
#10266=CARTESIAN_POINT('',(0.93,1.2,0.16));
#10267=CARTESIAN_POINT('',(0.57,1.2,0.16));
#10268=CARTESIAN_POINT('Origin',(0.57,0.,0.16));
#10269=CARTESIAN_POINT('',(0.885663593019381,-1.2,0.16));
#10270=CARTESIAN_POINT('',(0.885663593019381,0.,0.16));
#10271=CARTESIAN_POINT('',(0.93,-1.2,0.16));
#10272=CARTESIAN_POINT('',(0.93,0.,0.16));
#10273=CARTESIAN_POINT('',(0.57,-1.2,0.16));
#10274=CARTESIAN_POINT('Origin',(0.75,-1.2,0.));
#10275=CARTESIAN_POINT('',(0.885663593019381,-1.2,-0.16));
#10276=CARTESIAN_POINT('Origin',(0.,-1.2,0.));
#10277=CARTESIAN_POINT('',(0.93,-1.2,-0.16));
#10278=CARTESIAN_POINT('',(0.93,-1.2,0.16));
#10279=CARTESIAN_POINT('',(0.93,-1.2,-0.16));
#10280=CARTESIAN_POINT('Origin',(0.93,0.,-0.16));
#10281=CARTESIAN_POINT('',(0.885663593019381,0.,-0.16));
#10282=CARTESIAN_POINT('',(0.93,0.,-0.16));
#10283=CARTESIAN_POINT('Origin',(0.93,0.,0.16));
#10284=CARTESIAN_POINT('Origin',(1.05,1.5,0.));
#10285=CARTESIAN_POINT('',(-1.05,1.5,-1.28587913910472E-16));
#10286=CARTESIAN_POINT('Origin',(0.,1.5,0.));
#10287=CARTESIAN_POINT('',(-0.9,1.5,-1.10218211923262E-16));
#10288=CARTESIAN_POINT('Origin',(0.,1.5,0.));
#10289=CARTESIAN_POINT('Origin',(0.,1.315,0.));
#10290=CARTESIAN_POINT('',(-1.05,1.13,-1.28587913910472E-16));
#10291=CARTESIAN_POINT('Origin',(0.,1.13,0.));
#10292=CARTESIAN_POINT('',(-1.05,1.315,-1.28587913910472E-16));
#10293=CARTESIAN_POINT('Origin',(1.,1.13,0.));
#10294=CARTESIAN_POINT('',(-1.,1.13,-1.22464679914735E-16));
#10295=CARTESIAN_POINT('Origin',(0.,1.13,0.));
#10296=CARTESIAN_POINT('Origin',(0.,1.065,0.));
#10297=CARTESIAN_POINT('',(-1.,1.,-1.22464679914735E-16));
#10298=CARTESIAN_POINT('Origin',(0.,1.,0.));
#10299=CARTESIAN_POINT('',(-1.,1.065,-1.22464679914735E-16));
#10300=CARTESIAN_POINT('Origin',(1.05,1.,0.));
#10301=CARTESIAN_POINT('',(-1.05,1.,-1.28587913910472E-16));
#10302=CARTESIAN_POINT('Origin',(0.,1.,0.));
#10303=CARTESIAN_POINT('Origin',(0.,0.,0.));
#10304=CARTESIAN_POINT('',(-1.05,-1.,-1.28587913910472E-16));
#10305=CARTESIAN_POINT('Origin',(0.,-1.,0.));
#10306=CARTESIAN_POINT('',(-1.05,0.,-1.28587913910472E-16));
#10307=CARTESIAN_POINT('Origin',(1.,-1.,0.));
#10308=CARTESIAN_POINT('',(-1.,-1.,-1.22464679914735E-16));
#10309=CARTESIAN_POINT('Origin',(0.,-1.,0.));
#10310=CARTESIAN_POINT('Origin',(0.,-1.065,0.));
#10311=CARTESIAN_POINT('',(-1.,-1.13,-1.22464679914735E-16));
#10312=CARTESIAN_POINT('Origin',(0.,-1.13,0.));
#10313=CARTESIAN_POINT('',(-1.,-1.065,-1.22464679914735E-16));
#10314=CARTESIAN_POINT('Origin',(1.05,-1.13,0.));
#10315=CARTESIAN_POINT('',(-1.05,-1.13,-1.28587913910472E-16));
#10316=CARTESIAN_POINT('Origin',(0.,-1.13,0.));
#10317=CARTESIAN_POINT('Origin',(0.,-1.315,0.));
#10318=CARTESIAN_POINT('',(-1.05,-1.5,-1.28587913910472E-16));
#10319=CARTESIAN_POINT('Origin',(0.,-1.5,0.));
#10320=CARTESIAN_POINT('',(-1.05,-1.315,-1.28587913910472E-16));
#10321=CARTESIAN_POINT('Origin',(0.9,-1.5,0.));
#10322=CARTESIAN_POINT('',(-0.9,-1.5,-1.10218211923262E-16));
#10323=CARTESIAN_POINT('Origin',(0.,-1.5,0.));
#10324=CARTESIAN_POINT('Origin',(0.,0.,0.));
#10325=CARTESIAN_POINT('',(-0.9,0.,-1.10218211923262E-16));
#10326=CARTESIAN_POINT('',(0.,0.,0.));
#10327=CARTESIAN_POINT('Origin',(0.75,1.2,0.));
#10328=CARTESIAN_POINT('',(0.880582193778639,1.2,0.16));
#10329=CARTESIAN_POINT('',(0.880582193778639,1.2,-0.16));
#10330=CARTESIAN_POINT('Origin',(0.,1.2,0.));
#10331=CARTESIAN_POINT('',(0.583459510163302,1.2,0.16));
#10332=CARTESIAN_POINT('',(0.57,1.2,0.16));
#10333=CARTESIAN_POINT('',(0.583459510163302,1.2,-0.16));
#10334=CARTESIAN_POINT('Origin',(0.,1.2,0.));
#10335=CARTESIAN_POINT('',(0.93,1.2,-0.16));
#10336=CARTESIAN_POINT('Origin',(0.93,0.,-0.16));
#10337=CARTESIAN_POINT('',(0.880582193778639,-1.2,-0.16));
#10338=CARTESIAN_POINT('',(0.880582193778639,0.,-0.16));
#10339=CARTESIAN_POINT('',(0.583459510163302,-1.2,-0.16));
#10340=CARTESIAN_POINT('',(0.583459510163302,0.,-0.16));
#10341=CARTESIAN_POINT('',(0.93,-1.2,-0.16));
#10342=CARTESIAN_POINT('Origin',(0.75,-1.2,0.));
#10343=CARTESIAN_POINT('',(0.880582193778639,-1.2,0.16));
#10344=CARTESIAN_POINT('Origin',(0.,-1.2,0.));
#10345=CARTESIAN_POINT('',(0.583459510163302,-1.2,0.16));
#10346=CARTESIAN_POINT('Origin',(0.,-1.2,0.));
#10347=CARTESIAN_POINT('',(0.57,-1.2,0.16));
#10348=CARTESIAN_POINT('Origin',(0.57,0.,0.16));
#10349=CARTESIAN_POINT('',(0.880582193778639,0.,0.16));
#10350=CARTESIAN_POINT('',(0.583459510163302,0.,0.16));
#10351=CARTESIAN_POINT('Origin',(0.895,1.35,0.));
#10352=CARTESIAN_POINT('',(-0.895,1.35,-1.09605888523688E-16));
#10353=CARTESIAN_POINT('Origin',(0.,1.35,0.));
#10354=CARTESIAN_POINT('',(-0.605,1.35,-7.40911313484149E-17));
#10355=CARTESIAN_POINT('Origin',(0.,1.35,0.));
#10356=CARTESIAN_POINT('Origin',(0.,0.,0.));
#10357=CARTESIAN_POINT('',(-0.895,-1.35,-1.09605888523688E-16));
#10358=CARTESIAN_POINT('Origin',(0.,-1.35,0.));
#10359=CARTESIAN_POINT('',(-0.895,0.,-1.09605888523688E-16));
#10360=CARTESIAN_POINT('Origin',(0.605,-1.35,0.));
#10361=CARTESIAN_POINT('',(-0.605,-1.35,-7.40911313484149E-17));
#10362=CARTESIAN_POINT('Origin',(0.,-1.35,0.));
#10363=CARTESIAN_POINT('Origin',(0.,0.,0.));
#10364=CARTESIAN_POINT('',(-0.605,0.,-7.40911313484149E-17));
#10365=CARTESIAN_POINT('',(0.,0.,0.));
#10366=CARTESIAN_POINT('',(0.,0.,0.));
#10367=CARTESIAN_POINT('',(0.,0.,0.));
#10368=CARTESIAN_POINT('Origin',(8.1,3.2,2.8));
#10369=CARTESIAN_POINT('',(8.2,3.2,3.025));
#10370=CARTESIAN_POINT('Origin',(8.2,3.2,2.8));
#10371=CARTESIAN_POINT('',(8.5,3.2,3.025));
#10372=CARTESIAN_POINT('',(8.1,3.2,3.025));
#10373=CARTESIAN_POINT('Origin',(8.5,3.2,2.8));
#10374=CARTESIAN_POINT('Origin',(8.1,0.8,5.2));
#10375=CARTESIAN_POINT('',(8.2,0.8,5.425));
#10376=CARTESIAN_POINT('Origin',(8.2,0.8,5.2));
#10377=CARTESIAN_POINT('',(8.5,0.8,5.425));
#10378=CARTESIAN_POINT('',(8.1,0.8,5.425));
#10379=CARTESIAN_POINT('Origin',(8.5,0.8,5.2));
#10380=CARTESIAN_POINT('Origin',(8.1,0.8,2.8));
#10381=CARTESIAN_POINT('',(8.2,0.8,3.025));
#10382=CARTESIAN_POINT('Origin',(8.2,0.8,2.8));
#10383=CARTESIAN_POINT('',(8.5,0.8,3.025));
#10384=CARTESIAN_POINT('',(8.1,0.8,3.025));
#10385=CARTESIAN_POINT('Origin',(8.5,0.8,2.8));
#10386=CARTESIAN_POINT('Origin',(8.1,3.2,5.2));
#10387=CARTESIAN_POINT('',(8.2,3.2,5.425));
#10388=CARTESIAN_POINT('Origin',(8.2,3.2,5.2));
#10389=CARTESIAN_POINT('',(8.5,3.2,5.425));
#10390=CARTESIAN_POINT('',(8.1,3.2,5.425));
#10391=CARTESIAN_POINT('Origin',(8.5,3.2,5.2));
#10392=CARTESIAN_POINT('Origin',(8.1,2.,4.));
#10393=CARTESIAN_POINT('',(8.2,2.,4.7));
#10394=CARTESIAN_POINT('Origin',(8.2,2.,4.));
#10395=CARTESIAN_POINT('',(8.5,2.,4.7));
#10396=CARTESIAN_POINT('',(8.1,2.,4.7));
#10397=CARTESIAN_POINT('Origin',(8.5,2.,4.));
#10398=CARTESIAN_POINT('Origin',(8.5,3.7,2.3));
#10399=CARTESIAN_POINT('',(8.5,3.7,2.3));
#10400=CARTESIAN_POINT('',(8.2,3.7,2.3));
#10401=CARTESIAN_POINT('',(8.5,3.7,2.3));
#10402=CARTESIAN_POINT('',(8.2,3.7,5.7));
#10403=CARTESIAN_POINT('',(8.2,3.7,2.3));
#10404=CARTESIAN_POINT('',(8.5,3.7,5.7));
#10405=CARTESIAN_POINT('',(8.5,3.7,5.7));
#10406=CARTESIAN_POINT('',(8.5,3.7,2.3));
#10407=CARTESIAN_POINT('Origin',(8.5,0.3,2.3));
#10408=CARTESIAN_POINT('',(8.5,0.3,2.3));
#10409=CARTESIAN_POINT('',(8.5,0.3,2.3));
#10410=CARTESIAN_POINT('',(8.5,0.3,5.7));
#10411=CARTESIAN_POINT('',(8.5,0.3,5.7));
#10412=CARTESIAN_POINT('',(8.5,0.3,2.3));
#10413=CARTESIAN_POINT('Origin',(8.2,0.3,2.3));
#10414=CARTESIAN_POINT('',(8.2,0.3,2.3));
#10415=CARTESIAN_POINT('',(8.2,0.3,2.3));
#10416=CARTESIAN_POINT('',(8.2,0.3,5.7));
#10417=CARTESIAN_POINT('',(8.2,0.3,5.7));
#10418=CARTESIAN_POINT('',(8.2,0.3,2.3));
#10419=CARTESIAN_POINT('Origin',(8.2,3.7,2.3));
#10420=CARTESIAN_POINT('',(8.2,3.7,2.3));
#10421=CARTESIAN_POINT('',(8.2,3.7,5.7));
#10422=CARTESIAN_POINT('Origin',(8.35,2.,5.7));
#10423=CARTESIAN_POINT('Origin',(8.35,2.,2.3));
#10424=CARTESIAN_POINT('',(0.,0.,0.));
#10425=CARTESIAN_POINT('Origin',(0.,2.,9.6));
#10426=CARTESIAN_POINT('',(-0.305,2.,10.1));
#10427=CARTESIAN_POINT('Origin',(0.,2.,10.1));
#10428=CARTESIAN_POINT('',(-0.305,2.,9.6));
#10429=CARTESIAN_POINT('',(-0.305,2.,9.6));
#10430=CARTESIAN_POINT('Origin',(0.,2.,9.6));
#10431=CARTESIAN_POINT('Origin',(0.,2.,9.6));
#10432=CARTESIAN_POINT('',(-0.5,2.,10.1));
#10433=CARTESIAN_POINT('Origin',(0.,2.,10.1));
#10434=CARTESIAN_POINT('',(-0.5,2.,9.6));
#10435=CARTESIAN_POINT('',(-0.5,2.,9.6));
#10436=CARTESIAN_POINT('Origin',(0.,2.,9.6));
#10437=CARTESIAN_POINT('Origin',(0.,2.,10.1));
#10438=CARTESIAN_POINT('Origin',(0.,2.,9.6));
#10439=CARTESIAN_POINT('',(0.,0.,0.));
#10440=CARTESIAN_POINT('Origin',(0.,2.,10.1));
#10441=CARTESIAN_POINT('',(-0.225,2.,10.3));
#10442=CARTESIAN_POINT('Origin',(0.,2.,10.3));
#10443=CARTESIAN_POINT('',(-0.225,2.,10.1));
#10444=CARTESIAN_POINT('',(-0.225,2.,10.1));
#10445=CARTESIAN_POINT('Origin',(0.,2.,10.1));
#10446=CARTESIAN_POINT('Origin',(0.,2.,10.1));
#10447=CARTESIAN_POINT('',(-0.5,2.,10.3));
#10448=CARTESIAN_POINT('Origin',(0.,2.,10.3));
#10449=CARTESIAN_POINT('',(-0.5,2.,10.1));
#10450=CARTESIAN_POINT('',(-0.5,2.,10.1));
#10451=CARTESIAN_POINT('Origin',(0.,2.,10.1));
#10452=CARTESIAN_POINT('Origin',(0.,2.,10.3));
#10453=CARTESIAN_POINT('Origin',(0.,2.,10.1));
#10454=CARTESIAN_POINT('',(0.,0.,0.));
#10455=CARTESIAN_POINT('Origin',(0.0866025403784439,-0.4,-0.15));
#10456=CARTESIAN_POINT('',(0.173205080756888,-0.4,0.));
#10457=CARTESIAN_POINT('',(0.0866025403784439,-0.4,-0.15));
#10458=CARTESIAN_POINT('',(0.173205080756888,-0.4,0.));
#10459=CARTESIAN_POINT('',(0.0866025403784439,-0.64,-0.15));
#10460=CARTESIAN_POINT('',(0.0866025403784439,-0.4,-0.15));
#10461=CARTESIAN_POINT('',(0.173205080756888,-0.64,0.));
#10462=CARTESIAN_POINT('',(0.173205080756888,-0.64,0.));
#10463=CARTESIAN_POINT('',(0.173205080756888,-0.4,0.));
#10464=CARTESIAN_POINT('Origin',(-0.0866025403784438,-0.4,-0.15));
#10465=CARTESIAN_POINT('',(-0.0866025403784438,-0.4,-0.15));
#10466=CARTESIAN_POINT('',(0.0866025403784439,-0.4,-0.15));
#10467=CARTESIAN_POINT('',(-0.0866025403784438,-0.64,-0.15));
#10468=CARTESIAN_POINT('',(-0.0866025403784438,-0.4,-0.15));
#10469=CARTESIAN_POINT('',(0.0866025403784439,-0.64,-0.15));
#10470=CARTESIAN_POINT('Origin',(-0.173205080756888,-0.4,-2.77555756156289E-17));
#10471=CARTESIAN_POINT('',(-0.173205080756888,-0.4,-2.12115047744981E-17));
#10472=CARTESIAN_POINT('',(-0.0866025403784438,-0.4,-0.15));
#10473=CARTESIAN_POINT('',(-0.173205080756888,-0.64,-2.77555756156289E-17));
#10474=CARTESIAN_POINT('',(-0.173205080756888,-0.4,-2.12115047744981E-17));
#10475=CARTESIAN_POINT('',(-0.0866025403784438,-0.64,-0.15));
#10476=CARTESIAN_POINT('Origin',(-0.0866025403784439,-0.4,0.15));
#10477=CARTESIAN_POINT('',(-0.0866025403784439,-0.4,0.15));
#10478=CARTESIAN_POINT('',(-0.173205080756888,-0.4,-2.12115047744981E-17));
#10479=CARTESIAN_POINT('',(-0.0866025403784439,-0.64,0.15));
#10480=CARTESIAN_POINT('',(-0.0866025403784439,-0.4,0.15));
#10481=CARTESIAN_POINT('',(-0.173205080756888,-0.64,-2.12115047744981E-17));
#10482=CARTESIAN_POINT('Origin',(0.0866025403784439,-0.4,0.15));
#10483=CARTESIAN_POINT('',(0.0866025403784439,-0.4,0.15));
#10484=CARTESIAN_POINT('',(-0.0866025403784439,-0.4,0.15));
#10485=CARTESIAN_POINT('',(0.0866025403784439,-0.64,0.15));
#10486=CARTESIAN_POINT('',(0.0866025403784439,-0.4,0.15));
#10487=CARTESIAN_POINT('',(-0.0866025403784439,-0.64,0.15));
#10488=CARTESIAN_POINT('Origin',(0.173205080756888,-0.4,0.));
#10489=CARTESIAN_POINT('',(0.0866025403784439,-0.4,0.15));
#10490=CARTESIAN_POINT('',(0.0866025403784439,-0.64,0.15));
#10491=CARTESIAN_POINT('Origin',(0.,-0.4,-2.77555756156289E-17));
#10492=CARTESIAN_POINT('Origin',(0.,-0.64,-2.77555756156289E-17));
#10493=CARTESIAN_POINT('Origin',(0.,-1.,0.));
#10494=CARTESIAN_POINT('',(-0.1954,-1.,2.39295984553393E-17));
#10495=CARTESIAN_POINT('Origin',(0.,-1.,0.));
#10496=CARTESIAN_POINT('Origin',(0.3,0.4,0.));
#10497=CARTESIAN_POINT('',(-0.3,0.4,-3.67394039744206E-17));
#10498=CARTESIAN_POINT('Origin',(0.,0.4,0.));
#10499=CARTESIAN_POINT('Origin',(0.,0.375,0.));
#10500=CARTESIAN_POINT('',(-0.35,0.35,-4.28626379701573E-17));
#10501=CARTESIAN_POINT('Origin',(0.,0.35,0.));
#10502=CARTESIAN_POINT('',(-0.325,0.375,-3.9801020972289E-17));
#10503=CARTESIAN_POINT('Origin',(0.,0.19,0.));
#10504=CARTESIAN_POINT('',(-0.35,0.03,-4.28626379701574E-17));
#10505=CARTESIAN_POINT('Origin',(0.,0.03,0.));
#10506=CARTESIAN_POINT('',(-0.35,0.19,-4.28626379701574E-17));
#10507=CARTESIAN_POINT('Origin',(0.,0.0149999999999999,0.));
#10508=CARTESIAN_POINT('',(-0.32,-3.29597460435593E-17,-3.91886975727153E-17));
#10509=CARTESIAN_POINT('Origin',(0.,0.,0.));
#10510=CARTESIAN_POINT('',(-0.335,0.0149999999999999,-4.10256677714363E-17));
#10511=CARTESIAN_POINT('Origin',(0.22,0.,0.));
#10512=CARTESIAN_POINT('',(-0.22,-6.93889390390723E-18,-2.69422295812418E-17));
#10513=CARTESIAN_POINT('Origin',(0.,0.,0.));
#10514=CARTESIAN_POINT('Origin',(0.,-0.02,0.));
#10515=CARTESIAN_POINT('',(-0.1954,-0.0492,2.39295984553393E-17));
#10516=CARTESIAN_POINT('Origin',(0.,-0.0492,0.));
#10517=CARTESIAN_POINT('',(-0.21,-0.02,-2.57175827820944E-17));
#10518=CARTESIAN_POINT('Origin',(0.,-0.8,0.));
#10519=CARTESIAN_POINT('',(-0.1954,-0.8,-2.39295984553393E-17));
#10520=CARTESIAN_POINT('',(0.,0.,0.));
#10521=CARTESIAN_POINT('',(1.76776695296637,1.76776695296637,1.8));
#10522=CARTESIAN_POINT('',(-1.76776695296637,1.76776695296637,1.8));
#10523=CARTESIAN_POINT('',(-1.76776695296637,-1.76776695296637,1.8));
#10524=CARTESIAN_POINT('',(1.76776695296637,-1.76776695296637,1.8));
#10525=CARTESIAN_POINT('',(0.,0.,0.));
#10526=CARTESIAN_POINT('',(0.,0.,0.));
#10527=CARTESIAN_POINT('',(0.,0.,2.5));
#10528=CARTESIAN_POINT('',(1.23743686707646,1.23743686707646,4.));
#10529=CARTESIAN_POINT('',(-1.23743686707646,1.23743686707646,4.));
#10530=CARTESIAN_POINT('',(-1.23743686707646,-1.23743686707646,4.));
#10531=CARTESIAN_POINT('',(1.23743686707646,-1.23743686707646,4.));
#10532=CARTESIAN_POINT('',(3.5,4.,4.));
#10533=CARTESIAN_POINT('',(-1.5,2.,0.));
#10534=CARTESIAN_POINT('',(4.,2.9,2.));
#10535=CARTESIAN_POINT('',(4.,5.1,2.));
#10536=CARTESIAN_POINT('',(4.,4.,5.2));
#10537=CARTESIAN_POINT('',(5.5,2.,0.));
#10538=CARTESIAN_POINT('',(11.,2.9,2.));
#10539=CARTESIAN_POINT('',(11.,5.1,2.));
#10540=CARTESIAN_POINT('',(11.,4.,5.2));
#10541=CARTESIAN_POINT('',(0.,0.,0.));
#10542=CARTESIAN_POINT('',(0.,0.,0.));
#10543=CARTESIAN_POINT('',(0.,0.,0.));
#10544=CARTESIAN_POINT('',(0.,0.,0.));
#10545=CARTESIAN_POINT('',(-2.5,-2.5,4.8));
#10546=CARTESIAN_POINT('',(0.9,0.,1.4));
#10547=CARTESIAN_POINT('',(0.,0.,0.));
#10548=CARTESIAN_POINT('',(0.,0.,0.));
#10549=CARTESIAN_POINT('',(0.,0.,0.));
#10550=CARTESIAN_POINT('',(0.,0.,0.));
#10551=CARTESIAN_POINT('',(0.,2.,10.3));
#10552=CARTESIAN_POINT('',(0.,0.,0.));
#10553=CARTESIAN_POINT('',(0.,0.,0.));
#10554=CARTESIAN_POINT('',(-2.5,2.,0.));
#10555=CARTESIAN_POINT('',(7.5,4.,4.));
#10556=CARTESIAN_POINT('',(-2.5,2.,0.));
#10557=CARTESIAN_POINT('',(17.5,6.,0.));
#10558=CARTESIAN_POINT('',(5.7,2.8,2.8));
#10559=CARTESIAN_POINT('',(5.7,2.8,5.2));
#10560=CARTESIAN_POINT('',(5.7,5.2,2.8));
#10561=CARTESIAN_POINT('',(5.7,5.2,5.2));
#10562=CARTESIAN_POINT('',(9.3,2.8,2.8));
#10563=CARTESIAN_POINT('',(9.3,2.8,5.2));
#10564=CARTESIAN_POINT('',(9.3,5.2,2.8));
#10565=CARTESIAN_POINT('',(9.3,5.2,5.2));
#10566=CARTESIAN_POINT('',(7.5,2.,0.));
#10567=CARTESIAN_POINT('',(7.5,2.,0.));
#10568=CARTESIAN_POINT('',(7.5,4.,10.3));
#10569=CARTESIAN_POINT('',(0.,0.,0.));
#10570=CARTESIAN_POINT('',(-3.06161699786838E-16,-1.73333694994851E-31,
-4.44089209850063E-16));
#10571=CARTESIAN_POINT('',(-0.629986409604792,-0.11178449591778,-1.81864734773863E-14));
#10572=CARTESIAN_POINT('',(-0.690683467854789,-1.04551176721179E-17,-1.53080849893419E-16));
#10573=UNCERTAINTY_MEASURE_WITH_UNIT(LENGTH_MEASURE(0.001),#10651,
'DISTANCE_ACCURACY_VALUE',
'Maximum model space distance between geometric entities at asserted c
onnectivities');
#10574=UNCERTAINTY_MEASURE_WITH_UNIT(LENGTH_MEASURE(0.001),#10651,
'DISTANCE_ACCURACY_VALUE',
'Maximum model space distance between geometric entities at asserted c
onnectivities');
#10575=UNCERTAINTY_MEASURE_WITH_UNIT(LENGTH_MEASURE(0.001),#10651,
'DISTANCE_ACCURACY_VALUE',
'Maximum model space distance between geometric entities at asserted c
onnectivities');
#10576=UNCERTAINTY_MEASURE_WITH_UNIT(LENGTH_MEASURE(0.001),#10651,
'DISTANCE_ACCURACY_VALUE',
'Maximum model space distance between geometric entities at asserted c
onnectivities');
#10577=UNCERTAINTY_MEASURE_WITH_UNIT(LENGTH_MEASURE(0.001),#10651,
'DISTANCE_ACCURACY_VALUE',
'Maximum model space distance between geometric entities at asserted c
onnectivities');
#10578=UNCERTAINTY_MEASURE_WITH_UNIT(LENGTH_MEASURE(0.001),#10651,
'DISTANCE_ACCURACY_VALUE',
'Maximum model space distance between geometric entities at asserted c
onnectivities');
#10579=UNCERTAINTY_MEASURE_WITH_UNIT(LENGTH_MEASURE(0.001),#10651,
'DISTANCE_ACCURACY_VALUE',
'Maximum model space distance between geometric entities at asserted c
onnectivities');
#10580=UNCERTAINTY_MEASURE_WITH_UNIT(LENGTH_MEASURE(0.001),#10651,
'DISTANCE_ACCURACY_VALUE',
'Maximum model space distance between geometric entities at asserted c
onnectivities');
#10581=UNCERTAINTY_MEASURE_WITH_UNIT(LENGTH_MEASURE(0.001),#10651,
'DISTANCE_ACCURACY_VALUE',
'Maximum model space distance between geometric entities at asserted c
onnectivities');
#10582=UNCERTAINTY_MEASURE_WITH_UNIT(LENGTH_MEASURE(0.001),#10651,
'DISTANCE_ACCURACY_VALUE',
'Maximum model space distance between geometric entities at asserted c
onnectivities');
#10583=UNCERTAINTY_MEASURE_WITH_UNIT(LENGTH_MEASURE(0.001),#10651,
'DISTANCE_ACCURACY_VALUE',
'Maximum model space distance between geometric entities at asserted c
onnectivities');
#10584=UNCERTAINTY_MEASURE_WITH_UNIT(LENGTH_MEASURE(0.001),#10651,
'DISTANCE_ACCURACY_VALUE',
'Maximum model space distance between geometric entities at asserted c
onnectivities');
#10585=UNCERTAINTY_MEASURE_WITH_UNIT(LENGTH_MEASURE(0.001),#10651,
'DISTANCE_ACCURACY_VALUE',
'Maximum model space distance between geometric entities at asserted c
onnectivities');
#10586=UNCERTAINTY_MEASURE_WITH_UNIT(LENGTH_MEASURE(0.001),#10651,
'DISTANCE_ACCURACY_VALUE',
'Maximum model space distance between geometric entities at asserted c
onnectivities');
#10587=UNCERTAINTY_MEASURE_WITH_UNIT(LENGTH_MEASURE(0.001),#10651,
'DISTANCE_ACCURACY_VALUE',
'Maximum model space distance between geometric entities at asserted c
onnectivities');
#10588=UNCERTAINTY_MEASURE_WITH_UNIT(LENGTH_MEASURE(0.001),#10651,
'DISTANCE_ACCURACY_VALUE',
'Maximum model space distance between geometric entities at asserted c
onnectivities');
#10589=UNCERTAINTY_MEASURE_WITH_UNIT(LENGTH_MEASURE(0.001),#10651,
'DISTANCE_ACCURACY_VALUE',
'Maximum model space distance between geometric entities at asserted c
onnectivities');
#10590=UNCERTAINTY_MEASURE_WITH_UNIT(LENGTH_MEASURE(0.001),#10651,
'DISTANCE_ACCURACY_VALUE',
'Maximum model space distance between geometric entities at asserted c
onnectivities');
#10591=UNCERTAINTY_MEASURE_WITH_UNIT(LENGTH_MEASURE(0.001),#10651,
'DISTANCE_ACCURACY_VALUE',
'Maximum model space distance between geometric entities at asserted c
onnectivities');
#10592=UNCERTAINTY_MEASURE_WITH_UNIT(LENGTH_MEASURE(0.001),#10651,
'DISTANCE_ACCURACY_VALUE',
'Maximum model space distance between geometric entities at asserted c
onnectivities');
#10593=UNCERTAINTY_MEASURE_WITH_UNIT(LENGTH_MEASURE(0.001),#10651,
'DISTANCE_ACCURACY_VALUE',
'Maximum model space distance between geometric entities at asserted c
onnectivities');
#10594=UNCERTAINTY_MEASURE_WITH_UNIT(LENGTH_MEASURE(0.001),#10651,
'DISTANCE_ACCURACY_VALUE',
'Maximum model space distance between geometric entities at asserted c
onnectivities');
#10595=UNCERTAINTY_MEASURE_WITH_UNIT(LENGTH_MEASURE(0.001),#10651,
'DISTANCE_ACCURACY_VALUE',
'Maximum model space distance between geometric entities at asserted c
onnectivities');
#10596=UNCERTAINTY_MEASURE_WITH_UNIT(LENGTH_MEASURE(0.001),#10651,
'DISTANCE_ACCURACY_VALUE',
'Maximum model space distance between geometric entities at asserted c
onnectivities');
#10597=UNCERTAINTY_MEASURE_WITH_UNIT(LENGTH_MEASURE(0.001),#10651,
'DISTANCE_ACCURACY_VALUE',
'Maximum model space distance between geometric entities at asserted c
onnectivities');
#10598=UNCERTAINTY_MEASURE_WITH_UNIT(LENGTH_MEASURE(0.001),#10651,
'DISTANCE_ACCURACY_VALUE',
'Maximum model space distance between geometric entities at asserted c
onnectivities');
#10599=UNCERTAINTY_MEASURE_WITH_UNIT(LENGTH_MEASURE(0.001),#10651,
'DISTANCE_ACCURACY_VALUE',
'Maximum model space distance between geometric entities at asserted c
onnectivities');
#10600=UNCERTAINTY_MEASURE_WITH_UNIT(LENGTH_MEASURE(0.001),#10651,
'DISTANCE_ACCURACY_VALUE',
'Maximum model space distance between geometric entities at asserted c
onnectivities');
#10601=UNCERTAINTY_MEASURE_WITH_UNIT(LENGTH_MEASURE(0.001),#10651,
'DISTANCE_ACCURACY_VALUE',
'Maximum model space distance between geometric entities at asserted c
onnectivities');
#10602=UNCERTAINTY_MEASURE_WITH_UNIT(LENGTH_MEASURE(0.001),#10651,
'DISTANCE_ACCURACY_VALUE',
'Maximum model space distance between geometric entities at asserted c
onnectivities');
#10603=UNCERTAINTY_MEASURE_WITH_UNIT(LENGTH_MEASURE(0.001),#10651,
'DISTANCE_ACCURACY_VALUE',
'Maximum model space distance between geometric entities at asserted c
onnectivities');
#10604=UNCERTAINTY_MEASURE_WITH_UNIT(LENGTH_MEASURE(0.001),#10651,
'DISTANCE_ACCURACY_VALUE',
'Maximum model space distance between geometric entities at asserted c
onnectivities');
#10605=UNCERTAINTY_MEASURE_WITH_UNIT(LENGTH_MEASURE(0.001),#10651,
'DISTANCE_ACCURACY_VALUE',
'Maximum model space distance between geometric entities at asserted c
onnectivities');
#10606=UNCERTAINTY_MEASURE_WITH_UNIT(LENGTH_MEASURE(0.001),#10651,
'DISTANCE_ACCURACY_VALUE',
'Maximum model space distance between geometric entities at asserted c
onnectivities');
#10607=UNCERTAINTY_MEASURE_WITH_UNIT(LENGTH_MEASURE(0.001),#10651,
'DISTANCE_ACCURACY_VALUE',
'Maximum model space distance between geometric entities at asserted c
onnectivities');
#10608=UNCERTAINTY_MEASURE_WITH_UNIT(LENGTH_MEASURE(0.001),#10651,
'DISTANCE_ACCURACY_VALUE',
'Maximum model space distance between geometric entities at asserted c
onnectivities');
#10609=UNCERTAINTY_MEASURE_WITH_UNIT(LENGTH_MEASURE(0.001),#10651,
'DISTANCE_ACCURACY_VALUE',
'Maximum model space distance between geometric entities at asserted c
onnectivities');
#10610=UNCERTAINTY_MEASURE_WITH_UNIT(LENGTH_MEASURE(0.001),#10651,
'DISTANCE_ACCURACY_VALUE',
'Maximum model space distance between geometric entities at asserted c
onnectivities');
#10611=UNCERTAINTY_MEASURE_WITH_UNIT(LENGTH_MEASURE(0.001),#10651,
'DISTANCE_ACCURACY_VALUE',
'Maximum model space distance between geometric entities at asserted c
onnectivities');
#10612=(
GEOMETRIC_REPRESENTATION_CONTEXT(3)
GLOBAL_UNCERTAINTY_ASSIGNED_CONTEXT((#10573))
GLOBAL_UNIT_ASSIGNED_CONTEXT((#10651,#10653,#10654))
REPRESENTATION_CONTEXT('','3D')
);
#10613=(
GEOMETRIC_REPRESENTATION_CONTEXT(3)
GLOBAL_UNCERTAINTY_ASSIGNED_CONTEXT((#10574))
GLOBAL_UNIT_ASSIGNED_CONTEXT((#10651,#10653,#10654))
REPRESENTATION_CONTEXT('','3D')
);
#10614=(
GEOMETRIC_REPRESENTATION_CONTEXT(3)
GLOBAL_UNCERTAINTY_ASSIGNED_CONTEXT((#10575))
GLOBAL_UNIT_ASSIGNED_CONTEXT((#10651,#10653,#10654))
REPRESENTATION_CONTEXT('','3D')
);
#10615=(
GEOMETRIC_REPRESENTATION_CONTEXT(3)
GLOBAL_UNCERTAINTY_ASSIGNED_CONTEXT((#10576))
GLOBAL_UNIT_ASSIGNED_CONTEXT((#10651,#10653,#10654))
REPRESENTATION_CONTEXT('','3D')
);
#10616=(
GEOMETRIC_REPRESENTATION_CONTEXT(3)
GLOBAL_UNCERTAINTY_ASSIGNED_CONTEXT((#10577))
GLOBAL_UNIT_ASSIGNED_CONTEXT((#10651,#10653,#10654))
REPRESENTATION_CONTEXT('','3D')
);
#10617=(
GEOMETRIC_REPRESENTATION_CONTEXT(3)
GLOBAL_UNCERTAINTY_ASSIGNED_CONTEXT((#10578))
GLOBAL_UNIT_ASSIGNED_CONTEXT((#10651,#10653,#10654))
REPRESENTATION_CONTEXT('','3D')
);
#10618=(
GEOMETRIC_REPRESENTATION_CONTEXT(3)
GLOBAL_UNCERTAINTY_ASSIGNED_CONTEXT((#10579))
GLOBAL_UNIT_ASSIGNED_CONTEXT((#10651,#10653,#10654))
REPRESENTATION_CONTEXT('','3D')
);
#10619=(
GEOMETRIC_REPRESENTATION_CONTEXT(3)
GLOBAL_UNCERTAINTY_ASSIGNED_CONTEXT((#10580))
GLOBAL_UNIT_ASSIGNED_CONTEXT((#10651,#10653,#10654))
REPRESENTATION_CONTEXT('','3D')
);
#10620=(
GEOMETRIC_REPRESENTATION_CONTEXT(3)
GLOBAL_UNCERTAINTY_ASSIGNED_CONTEXT((#10581))
GLOBAL_UNIT_ASSIGNED_CONTEXT((#10651,#10653,#10654))
REPRESENTATION_CONTEXT('','3D')
);
#10621=(
GEOMETRIC_REPRESENTATION_CONTEXT(3)
GLOBAL_UNCERTAINTY_ASSIGNED_CONTEXT((#10582))
GLOBAL_UNIT_ASSIGNED_CONTEXT((#10651,#10653,#10654))
REPRESENTATION_CONTEXT('','3D')
);
#10622=(
GEOMETRIC_REPRESENTATION_CONTEXT(3)
GLOBAL_UNCERTAINTY_ASSIGNED_CONTEXT((#10583))
GLOBAL_UNIT_ASSIGNED_CONTEXT((#10651,#10653,#10654))
REPRESENTATION_CONTEXT('','3D')
);
#10623=(
GEOMETRIC_REPRESENTATION_CONTEXT(3)
GLOBAL_UNCERTAINTY_ASSIGNED_CONTEXT((#10584))
GLOBAL_UNIT_ASSIGNED_CONTEXT((#10651,#10653,#10654))
REPRESENTATION_CONTEXT('','3D')
);
#10624=(
GEOMETRIC_REPRESENTATION_CONTEXT(3)
GLOBAL_UNCERTAINTY_ASSIGNED_CONTEXT((#10585))
GLOBAL_UNIT_ASSIGNED_CONTEXT((#10651,#10653,#10654))
REPRESENTATION_CONTEXT('','3D')
);
#10625=(
GEOMETRIC_REPRESENTATION_CONTEXT(3)
GLOBAL_UNCERTAINTY_ASSIGNED_CONTEXT((#10586))
GLOBAL_UNIT_ASSIGNED_CONTEXT((#10651,#10653,#10654))
REPRESENTATION_CONTEXT('','3D')
);
#10626=(
GEOMETRIC_REPRESENTATION_CONTEXT(3)
GLOBAL_UNCERTAINTY_ASSIGNED_CONTEXT((#10587))
GLOBAL_UNIT_ASSIGNED_CONTEXT((#10651,#10653,#10654))
REPRESENTATION_CONTEXT('','3D')
);
#10627=(
GEOMETRIC_REPRESENTATION_CONTEXT(3)
GLOBAL_UNCERTAINTY_ASSIGNED_CONTEXT((#10588))
GLOBAL_UNIT_ASSIGNED_CONTEXT((#10651,#10653,#10654))
REPRESENTATION_CONTEXT('','3D')
);
#10628=(
GEOMETRIC_REPRESENTATION_CONTEXT(3)
GLOBAL_UNCERTAINTY_ASSIGNED_CONTEXT((#10589))
GLOBAL_UNIT_ASSIGNED_CONTEXT((#10651,#10653,#10654))
REPRESENTATION_CONTEXT('','3D')
);
#10629=(
GEOMETRIC_REPRESENTATION_CONTEXT(3)
GLOBAL_UNCERTAINTY_ASSIGNED_CONTEXT((#10590))
GLOBAL_UNIT_ASSIGNED_CONTEXT((#10651,#10653,#10654))
REPRESENTATION_CONTEXT('','3D')
);
#10630=(
GEOMETRIC_REPRESENTATION_CONTEXT(3)
GLOBAL_UNCERTAINTY_ASSIGNED_CONTEXT((#10591))
GLOBAL_UNIT_ASSIGNED_CONTEXT((#10651,#10653,#10654))
REPRESENTATION_CONTEXT('','3D')
);
#10631=(
GEOMETRIC_REPRESENTATION_CONTEXT(3)
GLOBAL_UNCERTAINTY_ASSIGNED_CONTEXT((#10592))
GLOBAL_UNIT_ASSIGNED_CONTEXT((#10651,#10653,#10654))
REPRESENTATION_CONTEXT('','3D')
);
#10632=(
GEOMETRIC_REPRESENTATION_CONTEXT(3)
GLOBAL_UNCERTAINTY_ASSIGNED_CONTEXT((#10593))
GLOBAL_UNIT_ASSIGNED_CONTEXT((#10651,#10653,#10654))
REPRESENTATION_CONTEXT('','3D')
);
#10633=(
GEOMETRIC_REPRESENTATION_CONTEXT(3)
GLOBAL_UNCERTAINTY_ASSIGNED_CONTEXT((#10594))
GLOBAL_UNIT_ASSIGNED_CONTEXT((#10651,#10653,#10654))
REPRESENTATION_CONTEXT('','3D')
);
#10634=(
GEOMETRIC_REPRESENTATION_CONTEXT(3)
GLOBAL_UNCERTAINTY_ASSIGNED_CONTEXT((#10595))
GLOBAL_UNIT_ASSIGNED_CONTEXT((#10651,#10653,#10654))
REPRESENTATION_CONTEXT('','3D')
);
#10635=(
GEOMETRIC_REPRESENTATION_CONTEXT(3)
GLOBAL_UNCERTAINTY_ASSIGNED_CONTEXT((#10596))
GLOBAL_UNIT_ASSIGNED_CONTEXT((#10651,#10653,#10654))
REPRESENTATION_CONTEXT('','3D')
);
#10636=(
GEOMETRIC_REPRESENTATION_CONTEXT(3)
GLOBAL_UNCERTAINTY_ASSIGNED_CONTEXT((#10597))
GLOBAL_UNIT_ASSIGNED_CONTEXT((#10651,#10653,#10654))
REPRESENTATION_CONTEXT('','3D')
);
#10637=(
GEOMETRIC_REPRESENTATION_CONTEXT(3)
GLOBAL_UNCERTAINTY_ASSIGNED_CONTEXT((#10598))
GLOBAL_UNIT_ASSIGNED_CONTEXT((#10651,#10653,#10654))
REPRESENTATION_CONTEXT('','3D')
);
#10638=(
GEOMETRIC_REPRESENTATION_CONTEXT(3)
GLOBAL_UNCERTAINTY_ASSIGNED_CONTEXT((#10599))
GLOBAL_UNIT_ASSIGNED_CONTEXT((#10651,#10653,#10654))
REPRESENTATION_CONTEXT('','3D')
);
#10639=(
GEOMETRIC_REPRESENTATION_CONTEXT(3)
GLOBAL_UNCERTAINTY_ASSIGNED_CONTEXT((#10600))
GLOBAL_UNIT_ASSIGNED_CONTEXT((#10651,#10653,#10654))
REPRESENTATION_CONTEXT('','3D')
);
#10640=(
GEOMETRIC_REPRESENTATION_CONTEXT(3)
GLOBAL_UNCERTAINTY_ASSIGNED_CONTEXT((#10601))
GLOBAL_UNIT_ASSIGNED_CONTEXT((#10651,#10653,#10654))
REPRESENTATION_CONTEXT('','3D')
);
#10641=(
GEOMETRIC_REPRESENTATION_CONTEXT(3)
GLOBAL_UNCERTAINTY_ASSIGNED_CONTEXT((#10602))
GLOBAL_UNIT_ASSIGNED_CONTEXT((#10651,#10653,#10654))
REPRESENTATION_CONTEXT('','3D')
);
#10642=(
GEOMETRIC_REPRESENTATION_CONTEXT(3)
GLOBAL_UNCERTAINTY_ASSIGNED_CONTEXT((#10603))
GLOBAL_UNIT_ASSIGNED_CONTEXT((#10651,#10653,#10654))
REPRESENTATION_CONTEXT('','3D')
);
#10643=(
GEOMETRIC_REPRESENTATION_CONTEXT(3)
GLOBAL_UNCERTAINTY_ASSIGNED_CONTEXT((#10604))
GLOBAL_UNIT_ASSIGNED_CONTEXT((#10651,#10653,#10654))
REPRESENTATION_CONTEXT('','3D')
);
#10644=(
GEOMETRIC_REPRESENTATION_CONTEXT(3)
GLOBAL_UNCERTAINTY_ASSIGNED_CONTEXT((#10605))
GLOBAL_UNIT_ASSIGNED_CONTEXT((#10651,#10653,#10654))
REPRESENTATION_CONTEXT('','3D')
);
#10645=(
GEOMETRIC_REPRESENTATION_CONTEXT(3)
GLOBAL_UNCERTAINTY_ASSIGNED_CONTEXT((#10606))
GLOBAL_UNIT_ASSIGNED_CONTEXT((#10651,#10653,#10654))
REPRESENTATION_CONTEXT('','3D')
);
#10646=(
GEOMETRIC_REPRESENTATION_CONTEXT(3)
GLOBAL_UNCERTAINTY_ASSIGNED_CONTEXT((#10607))
GLOBAL_UNIT_ASSIGNED_CONTEXT((#10651,#10653,#10654))
REPRESENTATION_CONTEXT('','3D')
);
#10647=(
GEOMETRIC_REPRESENTATION_CONTEXT(3)
GLOBAL_UNCERTAINTY_ASSIGNED_CONTEXT((#10608))
GLOBAL_UNIT_ASSIGNED_CONTEXT((#10651,#10653,#10654))
REPRESENTATION_CONTEXT('','3D')
);
#10648=(
GEOMETRIC_REPRESENTATION_CONTEXT(3)
GLOBAL_UNCERTAINTY_ASSIGNED_CONTEXT((#10609))
GLOBAL_UNIT_ASSIGNED_CONTEXT((#10651,#10653,#10654))
REPRESENTATION_CONTEXT('','3D')
);
#10649=(
GEOMETRIC_REPRESENTATION_CONTEXT(3)
GLOBAL_UNCERTAINTY_ASSIGNED_CONTEXT((#10610))
GLOBAL_UNIT_ASSIGNED_CONTEXT((#10651,#10653,#10654))
REPRESENTATION_CONTEXT('','3D')
);
#10650=(
GEOMETRIC_REPRESENTATION_CONTEXT(3)
GLOBAL_UNCERTAINTY_ASSIGNED_CONTEXT((#10611))
GLOBAL_UNIT_ASSIGNED_CONTEXT((#10651,#10653,#10654))
REPRESENTATION_CONTEXT('','3D')
);
#10651=(
LENGTH_UNIT()
NAMED_UNIT(*)
SI_UNIT(.CENTI.,.METRE.)
);
#10652=(
LENGTH_UNIT()
NAMED_UNIT(*)
SI_UNIT($,.METRE.)
);
#10653=(
NAMED_UNIT(*)
PLANE_ANGLE_UNIT()
SI_UNIT($,.RADIAN.)
);
#10654=(
NAMED_UNIT(*)
SI_UNIT($,.STERADIAN.)
SOLID_ANGLE_UNIT()
);
#10655=SHAPE_DEFINITION_REPRESENTATION(#10693,#10794);
#10656=SHAPE_DEFINITION_REPRESENTATION(#10694,#10795);
#10657=SHAPE_DEFINITION_REPRESENTATION(#10695,#10796);
#10658=SHAPE_DEFINITION_REPRESENTATION(#10696,#10797);
#10659=SHAPE_DEFINITION_REPRESENTATION(#10697,#10798);
#10660=SHAPE_DEFINITION_REPRESENTATION(#10698,#10799);
#10661=SHAPE_DEFINITION_REPRESENTATION(#10699,#10800);
#10662=SHAPE_DEFINITION_REPRESENTATION(#10700,#10801);
#10663=SHAPE_DEFINITION_REPRESENTATION(#10701,#10802);
#10664=SHAPE_DEFINITION_REPRESENTATION(#10702,#10803);
#10665=SHAPE_DEFINITION_REPRESENTATION(#10703,#10804);
#10666=SHAPE_DEFINITION_REPRESENTATION(#10704,#10805);
#10667=SHAPE_DEFINITION_REPRESENTATION(#10710,#10806);
#10668=SHAPE_DEFINITION_REPRESENTATION(#10711,#10807);
#10669=SHAPE_DEFINITION_REPRESENTATION(#10712,#10808);
#10670=SHAPE_DEFINITION_REPRESENTATION(#10713,#10809);
#10671=SHAPE_DEFINITION_REPRESENTATION(#10714,#10810);
#10672=SHAPE_DEFINITION_REPRESENTATION(#10715,#10811);
#10673=SHAPE_DEFINITION_REPRESENTATION(#10716,#10812);
#10674=SHAPE_DEFINITION_REPRESENTATION(#10717,#10813);
#10675=SHAPE_DEFINITION_REPRESENTATION(#10718,#10814);
#10676=SHAPE_DEFINITION_REPRESENTATION(#10719,#10815);
#10677=SHAPE_DEFINITION_REPRESENTATION(#10720,#10816);
#10678=SHAPE_DEFINITION_REPRESENTATION(#10721,#10817);
#10679=SHAPE_DEFINITION_REPRESENTATION(#10722,#10818);
#10680=SHAPE_DEFINITION_REPRESENTATION(#10723,#10819);
#10681=SHAPE_DEFINITION_REPRESENTATION(#10724,#10820);
#10682=SHAPE_DEFINITION_REPRESENTATION(#10728,#10821);
#10683=SHAPE_DEFINITION_REPRESENTATION(#10729,#10822);
#10684=SHAPE_DEFINITION_REPRESENTATION(#10730,#10823);
#10685=SHAPE_DEFINITION_REPRESENTATION(#10731,#10824);
#10686=SHAPE_DEFINITION_REPRESENTATION(#10732,#10825);
#10687=SHAPE_DEFINITION_REPRESENTATION(#10733,#10826);
#10688=SHAPE_DEFINITION_REPRESENTATION(#10734,#10827);
#10689=SHAPE_DEFINITION_REPRESENTATION(#10737,#10828);
#10690=SHAPE_DEFINITION_REPRESENTATION(#10738,#10829);
#10691=SHAPE_DEFINITION_REPRESENTATION(#10739,#10830);
#10692=SHAPE_DEFINITION_REPRESENTATION(#10740,#10831);
#10693=PRODUCT_DEFINITION_SHAPE('',$,#10833);
#10694=PRODUCT_DEFINITION_SHAPE('',$,#10834);
#10695=PRODUCT_DEFINITION_SHAPE('',$,#10835);
#10696=PRODUCT_DEFINITION_SHAPE('',$,#10836);
#10697=PRODUCT_DEFINITION_SHAPE('',$,#10837);
#10698=PRODUCT_DEFINITION_SHAPE('',$,#10838);
#10699=PRODUCT_DEFINITION_SHAPE('',$,#10839);
#10700=PRODUCT_DEFINITION_SHAPE('',$,#10840);
#10701=PRODUCT_DEFINITION_SHAPE('',$,#10841);
#10702=PRODUCT_DEFINITION_SHAPE('',$,#10842);
#10703=PRODUCT_DEFINITION_SHAPE('',$,#10843);
#10704=PRODUCT_DEFINITION_SHAPE('',$,#10844);
#10705=PRODUCT_DEFINITION_SHAPE($,$,#200);
#10706=PRODUCT_DEFINITION_SHAPE($,$,#201);
#10707=PRODUCT_DEFINITION_SHAPE($,$,#202);
#10708=PRODUCT_DEFINITION_SHAPE($,$,#203);
#10709=PRODUCT_DEFINITION_SHAPE($,$,#204);
#10710=PRODUCT_DEFINITION_SHAPE('',$,#10845);
#10711=PRODUCT_DEFINITION_SHAPE('',$,#10846);
#10712=PRODUCT_DEFINITION_SHAPE('',$,#10847);
#10713=PRODUCT_DEFINITION_SHAPE('',$,#10848);
#10714=PRODUCT_DEFINITION_SHAPE('',$,#10849);
#10715=PRODUCT_DEFINITION_SHAPE('',$,#10850);
#10716=PRODUCT_DEFINITION_SHAPE('',$,#10851);
#10717=PRODUCT_DEFINITION_SHAPE('',$,#10852);
#10718=PRODUCT_DEFINITION_SHAPE('',$,#10853);
#10719=PRODUCT_DEFINITION_SHAPE('',$,#10854);
#10720=PRODUCT_DEFINITION_SHAPE('',$,#10855);
#10721=PRODUCT_DEFINITION_SHAPE('',$,#10856);
#10722=PRODUCT_DEFINITION_SHAPE('',$,#10857);
#10723=PRODUCT_DEFINITION_SHAPE('',$,#10858);
#10724=PRODUCT_DEFINITION_SHAPE('',$,#10859);
#10725=PRODUCT_DEFINITION_SHAPE($,$,#205);
#10726=PRODUCT_DEFINITION_SHAPE($,$,#206);
#10727=PRODUCT_DEFINITION_SHAPE($,$,#207);
#10728=PRODUCT_DEFINITION_SHAPE('',$,#10860);
#10729=PRODUCT_DEFINITION_SHAPE('',$,#10861);
#10730=PRODUCT_DEFINITION_SHAPE('',$,#10862);
#10731=PRODUCT_DEFINITION_SHAPE('',$,#10863);
#10732=PRODUCT_DEFINITION_SHAPE('',$,#10864);
#10733=PRODUCT_DEFINITION_SHAPE('',$,#10865);
#10734=PRODUCT_DEFINITION_SHAPE('',$,#10866);
#10735=PRODUCT_DEFINITION_SHAPE($,$,#208);
#10736=PRODUCT_DEFINITION_SHAPE($,$,#209);
#10737=PRODUCT_DEFINITION_SHAPE('',$,#10867);
#10738=PRODUCT_DEFINITION_SHAPE('',$,#10868);
#10739=PRODUCT_DEFINITION_SHAPE('',$,#10869);
#10740=PRODUCT_DEFINITION_SHAPE('',$,#10870);
#10741=PRODUCT_DEFINITION_SHAPE($,$,#210);
#10742=PRODUCT_DEFINITION_SHAPE($,$,#211);
#10743=PRODUCT_DEFINITION_SHAPE($,$,#212);
#10744=PRODUCT_DEFINITION_SHAPE($,$,#213);
#10745=PRODUCT_DEFINITION_SHAPE($,$,#214);
#10746=PRODUCT_DEFINITION_SHAPE($,$,#215);
#10747=PRODUCT_DEFINITION_SHAPE($,$,#216);
#10748=PRODUCT_DEFINITION_SHAPE($,$,#217);
#10749=PRODUCT_DEFINITION_SHAPE($,$,#218);
#10750=PRODUCT_DEFINITION_SHAPE($,$,#219);
#10751=PRODUCT_DEFINITION_SHAPE($,$,#220);
#10752=PRODUCT_DEFINITION_SHAPE($,$,#221);
#10753=PRODUCT_DEFINITION_SHAPE($,$,#222);
#10754=PRODUCT_DEFINITION_SHAPE($,$,#223);
#10755=PRODUCT_DEFINITION_SHAPE($,$,#224);
#10756=PRODUCT_DEFINITION_SHAPE($,$,#225);
#10757=PRODUCT_DEFINITION_SHAPE($,$,#226);
#10758=PRODUCT_DEFINITION_SHAPE($,$,#227);
#10759=PRODUCT_DEFINITION_SHAPE($,$,#228);
#10760=PRODUCT_DEFINITION_SHAPE($,$,#229);
#10761=PRODUCT_DEFINITION_SHAPE($,$,#230);
#10762=PRODUCT_DEFINITION_SHAPE($,$,#231);
#10763=PRODUCT_DEFINITION_SHAPE($,$,#232);
#10764=PRODUCT_DEFINITION_SHAPE($,$,#233);
#10765=PRODUCT_DEFINITION_SHAPE($,$,#234);
#10766=PRODUCT_DEFINITION_SHAPE($,$,#235);
#10767=PRODUCT_DEFINITION_SHAPE($,$,#236);
#10768=PRODUCT_DEFINITION_SHAPE($,$,#237);
#10769=PRODUCT_DEFINITION_SHAPE($,$,#238);
#10770=PRODUCT_DEFINITION_SHAPE($,$,#239);
#10771=PRODUCT_DEFINITION_SHAPE($,$,#240);
#10772=PRODUCT_DEFINITION_SHAPE($,$,#241);
#10773=PRODUCT_DEFINITION_SHAPE($,$,#242);
#10774=PRODUCT_DEFINITION_SHAPE($,$,#243);
#10775=PRODUCT_DEFINITION_SHAPE($,$,#244);
#10776=PRODUCT_DEFINITION_SHAPE($,$,#245);
#10777=PRODUCT_DEFINITION_SHAPE($,$,#246);
#10778=PRODUCT_DEFINITION_SHAPE($,$,#247);
#10779=PRODUCT_DEFINITION_SHAPE($,$,#248);
#10780=PRODUCT_DEFINITION_SHAPE($,$,#249);
#10781=PRODUCT_DEFINITION_SHAPE($,$,#250);
#10782=PRODUCT_DEFINITION_SHAPE($,$,#251);
#10783=PRODUCT_DEFINITION_SHAPE($,$,#252);
#10784=PRODUCT_DEFINITION_SHAPE($,$,#253);
#10785=PRODUCT_DEFINITION_SHAPE($,$,#254);
#10786=PRODUCT_DEFINITION_SHAPE($,$,#255);
#10787=PRODUCT_DEFINITION_SHAPE($,$,#256);
#10788=PRODUCT_DEFINITION_SHAPE($,$,#257);
#10789=PRODUCT_DEFINITION_SHAPE($,$,#258);
#10790=PRODUCT_DEFINITION_SHAPE($,$,#259);
#10791=PRODUCT_DEFINITION_SHAPE($,$,#260);
#10792=PRODUCT_DEFINITION_SHAPE($,$,#261);
#10793=PRODUCT_DEFINITION_SHAPE($,$,#262);
#10794=SHAPE_REPRESENTATION('',(#5915,#6667,#6668,#6669,#6670),#10612);
#10795=SHAPE_REPRESENTATION('',(#5916,#6618,#6619,#6620,#6621,#6622,#6623,
#6624,#6625,#6626,#6627,#6628,#6629,#6630,#6631,#6632,#6633,#6634,#6635,
#6636,#6637,#6638),#10613);
#10796=SHAPE_REPRESENTATION('',(#5917),#10614);
#10797=SHAPE_REPRESENTATION('',(#5948),#10615);
#10798=SHAPE_REPRESENTATION('',(#5972),#10616);
#10799=SHAPE_REPRESENTATION('',(#6042),#10617);
#10800=SHAPE_REPRESENTATION('',(#6083,#6212,#6213,#6214,#6215,#6216),#10618);
#10801=SHAPE_REPRESENTATION('',(#6084),#10619);
#10802=SHAPE_REPRESENTATION('',(#6104),#10620);
#10803=SHAPE_REPRESENTATION('',(#6124),#10621);
#10804=SHAPE_REPRESENTATION('',(#6141),#10622);
#10805=SHAPE_REPRESENTATION('',(#6195),#10623);
#10806=SHAPE_REPRESENTATION('',(#6217),#10624);
#10807=SHAPE_REPRESENTATION('',(#6225),#10625);
#10808=SHAPE_REPRESENTATION('',(#6255),#10626);
#10809=SHAPE_REPRESENTATION('',(#6272,#6639,#6640,#6641,#6642,#6643,#6644,
#6645,#6646,#6647,#6648,#6649),#10627);
#10810=SHAPE_REPRESENTATION('',(#6273),#10628);
#10811=SHAPE_REPRESENTATION('',(#6317),#10629);
#10812=SHAPE_REPRESENTATION('',(#6327),#10630);
#10813=SHAPE_REPRESENTATION('',(#6336),#10631);
#10814=SHAPE_REPRESENTATION('',(#6350),#10632);
#10815=SHAPE_REPRESENTATION('',(#6376),#10633);
#10816=SHAPE_REPRESENTATION('',(#6391),#10634);
#10817=SHAPE_REPRESENTATION('',(#6409),#10635);
#10818=SHAPE_REPRESENTATION('',(#6418,#6445,#6446,#6447),#10636);
#10819=SHAPE_REPRESENTATION('',(#6419),#10637);
#10820=SHAPE_REPRESENTATION('',(#6436),#10638);
#10821=SHAPE_REPRESENTATION('',(#6448,#6650,#6651,#6652,#6653,#6654,#6655,
#6656,#6657,#6658,#6659,#6660,#6661,#6662,#6663,#6664,#6665,#6666),#10639);
#10822=SHAPE_REPRESENTATION('',(#6449),#10640);
#10823=SHAPE_REPRESENTATION('',(#6467),#10641);
#10824=SHAPE_REPRESENTATION('',(#6476),#10642);
#10825=SHAPE_REPRESENTATION('',(#6502,#6552,#6553),#10643);
#10826=SHAPE_REPRESENTATION('',(#6503),#10644);
#10827=SHAPE_REPRESENTATION('',(#6535),#10645);
#10828=SHAPE_REPRESENTATION('',(#6554),#10646);
#10829=SHAPE_REPRESENTATION('',(#6576),#10647);
#10830=SHAPE_REPRESENTATION('',(#6585),#10648);
#10831=SHAPE_REPRESENTATION('',(#6594),#10649);
#10832=PRODUCT_DEFINITION_CONTEXT('part definition',#10948,'design');
#10833=PRODUCT_DEFINITION('PAT-096',
'PAT-096',#10871,#10832);
#10834=PRODUCT_DEFINITION('Base and guide','Base and guide',#10872,#10832);
#10835=PRODUCT_DEFINITION('Demonstrator base','Demonstrator base',#10873,
#10832);
#10836=PRODUCT_DEFINITION('M5x14 Cap Screw','M5x14 Cap Screw',#10874,#10832);
#10837=PRODUCT_DEFINITION('Pivot pedestal','Pivot pedestal',#10875,#10832);
#10838=PRODUCT_DEFINITION('Pivot cap','Pivot cap',#10876,#10832);
#10839=PRODUCT_DEFINITION('Sealed Ball Bearing - 10 x 30 x 9 mm',
'Sealed Ball Bearing - 10 x 30 x 9 mm',#10877,#10832);
#10840=PRODUCT_DEFINITION('Inner ring','Inner ring',#10878,#10832);
#10841=PRODUCT_DEFINITION('Outer ring','Outer ring',#10879,#10832);
#10842=PRODUCT_DEFINITION('Balls','Balls',#10880,#10832);
#10843=PRODUCT_DEFINITION('Cage','Cage',#10881,#10832);
#10844=PRODUCT_DEFINITION('Seals 2RS','Seals 2RS',#10882,#10832);
#10845=PRODUCT_DEFINITION('Eighty millimetre guide shaft',
'Eighty millimetre guide shaft',#10883,#10832);
#10846=PRODUCT_DEFINITION('Horizontal shaft support',
'Horizontal shaft support',#10884,#10832);
#10847=PRODUCT_DEFINITION('Socket Set Screw - M4x6',
'Socket Set Screw - M4x6',#10885,#10832);
#10848=PRODUCT_DEFINITION('Bell crank','Bell crank',#10886,#10832);
#10849=PRODUCT_DEFINITION('Bell crank and spindle',
'Bell crank and spindle',#10887,#10832);
#10850=PRODUCT_DEFINITION('Input grip','Input grip',#10888,#10832);
#10851=PRODUCT_DEFINITION('Lower race sleeve','Lower race sleeve',#10889,
#10832);
#10852=PRODUCT_DEFINITION('Spindle collar','Spindle collar',#10890,#10832);
#10853=PRODUCT_DEFINITION('Cap Screw - M4x16','Cap Screw - M4x16',#10891,
#10832);
#10854=PRODUCT_DEFINITION('M4x4 collar screw','M4x4 collar screw',#10892,
#10832);
#10855=PRODUCT_DEFINITION('Horizontal link pin','Horizontal link pin',#10893,
#10832);
#10856=PRODUCT_DEFINITION('Horizontal lower pin sleeve',
'Horizontal lower pin sleeve',#10894,#10832);
#10857=PRODUCT_DEFINITION('Connecting link','Connecting link',#10895,#10832);
#10858=PRODUCT_DEFINITION('Offset connecting link',
'Offset connecting link',#10896,#10832);
#10859=PRODUCT_DEFINITION('Plain link bushing','Plain link bushing',#10897,
#10832);
#10860=PRODUCT_DEFINITION('Output slider','Output slider',#10898,#10832);
#10861=PRODUCT_DEFINITION('Carriage link pin','Carriage link pin',#10899,
#10832);
#10862=PRODUCT_DEFINITION('Carriage pin sleeve','Carriage pin sleeve',#10900,
#10832);
#10863=PRODUCT_DEFINITION('Horizontal output housing',
'Horizontal output housing',#10901,#10832);
#10864=PRODUCT_DEFINITION('Linear Ball Bushing - 12 x 21 x 30 mm',
'Linear Ball Bushing - 12 x 21 x 30 mm',#10902,#10832);
#10865=PRODUCT_DEFINITION('Steel sleeve','Steel sleeve',#10903,#10832);
#10866=PRODUCT_DEFINITION('Ball retainer (plastic)',
'Ball retainer (plastic)',#10904,#10832);
#10867=PRODUCT_DEFINITION('Horizontal guide cap','Horizontal guide cap',
#10905,#10832);
#10868=PRODUCT_DEFINITION('Upper pin sleeve','Upper pin sleeve',#10906,
#10832);
#10869=PRODUCT_DEFINITION('Pin keeper','Pin keeper',#10907,#10832);
#10870=PRODUCT_DEFINITION('M4x10 Cap Screw','M4x10 Cap Screw',#10908,#10832);
#10871=PRODUCT_DEFINITION_FORMATION('',$,#10950);
#10872=PRODUCT_DEFINITION_FORMATION('',$,#10951);
#10873=PRODUCT_DEFINITION_FORMATION('',$,#10952);
#10874=PRODUCT_DEFINITION_FORMATION('',$,#10953);
#10875=PRODUCT_DEFINITION_FORMATION('',$,#10954);
#10876=PRODUCT_DEFINITION_FORMATION('',$,#10955);
#10877=PRODUCT_DEFINITION_FORMATION('',$,#10956);
#10878=PRODUCT_DEFINITION_FORMATION('',$,#10957);
#10879=PRODUCT_DEFINITION_FORMATION('',$,#10958);
#10880=PRODUCT_DEFINITION_FORMATION('',$,#10959);
#10881=PRODUCT_DEFINITION_FORMATION('',$,#10960);
#10882=PRODUCT_DEFINITION_FORMATION('',$,#10961);
#10883=PRODUCT_DEFINITION_FORMATION('',$,#10962);
#10884=PRODUCT_DEFINITION_FORMATION('',$,#10963);
#10885=PRODUCT_DEFINITION_FORMATION('',$,#10964);
#10886=PRODUCT_DEFINITION_FORMATION('',$,#10965);
#10887=PRODUCT_DEFINITION_FORMATION('',$,#10966);
#10888=PRODUCT_DEFINITION_FORMATION('',$,#10967);
#10889=PRODUCT_DEFINITION_FORMATION('',$,#10968);
#10890=PRODUCT_DEFINITION_FORMATION('',$,#10969);
#10891=PRODUCT_DEFINITION_FORMATION('',$,#10970);
#10892=PRODUCT_DEFINITION_FORMATION('',$,#10971);
#10893=PRODUCT_DEFINITION_FORMATION('',$,#10972);
#10894=PRODUCT_DEFINITION_FORMATION('',$,#10973);
#10895=PRODUCT_DEFINITION_FORMATION('',$,#10974);
#10896=PRODUCT_DEFINITION_FORMATION('',$,#10975);
#10897=PRODUCT_DEFINITION_FORMATION('',$,#10976);
#10898=PRODUCT_DEFINITION_FORMATION('',$,#10977);
#10899=PRODUCT_DEFINITION_FORMATION('',$,#10978);
#10900=PRODUCT_DEFINITION_FORMATION('',$,#10979);
#10901=PRODUCT_DEFINITION_FORMATION('',$,#10980);
#10902=PRODUCT_DEFINITION_FORMATION('',$,#10981);
#10903=PRODUCT_DEFINITION_FORMATION('',$,#10982);
#10904=PRODUCT_DEFINITION_FORMATION('',$,#10983);
#10905=PRODUCT_DEFINITION_FORMATION('',$,#10984);
#10906=PRODUCT_DEFINITION_FORMATION('',$,#10985);
#10907=PRODUCT_DEFINITION_FORMATION('',$,#10986);
#10908=PRODUCT_DEFINITION_FORMATION('',$,#10987);
#10909=PRODUCT_RELATED_PRODUCT_CATEGORY('PAT-096',
'PAT-096',(#10950));
#10910=PRODUCT_RELATED_PRODUCT_CATEGORY('Base and guide',
'Base and guide',(#10951));
#10911=PRODUCT_RELATED_PRODUCT_CATEGORY('Demonstrator base',
'Demonstrator base',(#10952));
#10912=PRODUCT_RELATED_PRODUCT_CATEGORY('M5x14 Cap Screw',
'M5x14 Cap Screw',(#10953));
#10913=PRODUCT_RELATED_PRODUCT_CATEGORY('Pivot pedestal',
'Pivot pedestal',(#10954));
#10914=PRODUCT_RELATED_PRODUCT_CATEGORY('Pivot cap','Pivot cap',(#10955));
#10915=PRODUCT_RELATED_PRODUCT_CATEGORY(
'Sealed Ball Bearing - 10 x 30 x 9 mm',
'Sealed Ball Bearing - 10 x 30 x 9 mm',(#10956));
#10916=PRODUCT_RELATED_PRODUCT_CATEGORY('Inner ring','Inner ring',(#10957));
#10917=PRODUCT_RELATED_PRODUCT_CATEGORY('Outer ring','Outer ring',(#10958));
#10918=PRODUCT_RELATED_PRODUCT_CATEGORY('Balls','Balls',(#10959));
#10919=PRODUCT_RELATED_PRODUCT_CATEGORY('Cage','Cage',(#10960));
#10920=PRODUCT_RELATED_PRODUCT_CATEGORY('Seals 2RS','Seals 2RS',(#10961));
#10921=PRODUCT_RELATED_PRODUCT_CATEGORY('Eighty millimetre guide shaft',
'Eighty millimetre guide shaft',(#10962));
#10922=PRODUCT_RELATED_PRODUCT_CATEGORY('Horizontal shaft support',
'Horizontal shaft support',(#10963));
#10923=PRODUCT_RELATED_PRODUCT_CATEGORY('Socket Set Screw - M4x6',
'Socket Set Screw - M4x6',(#10964));
#10924=PRODUCT_RELATED_PRODUCT_CATEGORY('Bell crank','Bell crank',(#10965));
#10925=PRODUCT_RELATED_PRODUCT_CATEGORY('Bell crank and spindle',
'Bell crank and spindle',(#10966));
#10926=PRODUCT_RELATED_PRODUCT_CATEGORY('Input grip','Input grip',(#10967));
#10927=PRODUCT_RELATED_PRODUCT_CATEGORY('Lower race sleeve',
'Lower race sleeve',(#10968));
#10928=PRODUCT_RELATED_PRODUCT_CATEGORY('Spindle collar',
'Spindle collar',(#10969));
#10929=PRODUCT_RELATED_PRODUCT_CATEGORY('Cap Screw - M4x16',
'Cap Screw - M4x16',(#10970));
#10930=PRODUCT_RELATED_PRODUCT_CATEGORY('M4x4 collar screw',
'M4x4 collar screw',(#10971));
#10931=PRODUCT_RELATED_PRODUCT_CATEGORY('Horizontal link pin',
'Horizontal link pin',(#10972));
#10932=PRODUCT_RELATED_PRODUCT_CATEGORY('Horizontal lower pin sleeve',
'Horizontal lower pin sleeve',(#10973));
#10933=PRODUCT_RELATED_PRODUCT_CATEGORY('Connecting link',
'Connecting link',(#10974));
#10934=PRODUCT_RELATED_PRODUCT_CATEGORY('Offset connecting link',
'Offset connecting link',(#10975));
#10935=PRODUCT_RELATED_PRODUCT_CATEGORY('Plain link bushing',
'Plain link bushing',(#10976));
#10936=PRODUCT_RELATED_PRODUCT_CATEGORY('Output slider','Output slider',
(#10977));
#10937=PRODUCT_RELATED_PRODUCT_CATEGORY('Carriage link pin',
'Carriage link pin',(#10978));
#10938=PRODUCT_RELATED_PRODUCT_CATEGORY('Carriage pin sleeve',
'Carriage pin sleeve',(#10979));
#10939=PRODUCT_RELATED_PRODUCT_CATEGORY('Horizontal output housing',
'Horizontal output housing',(#10980));
#10940=PRODUCT_RELATED_PRODUCT_CATEGORY(
'Linear Ball Bushing - 12 x 21 x 30 mm',
'Linear Ball Bushing - 12 x 21 x 30 mm',(#10981));
#10941=PRODUCT_RELATED_PRODUCT_CATEGORY('Steel sleeve','Steel sleeve',(#10982));
#10942=PRODUCT_RELATED_PRODUCT_CATEGORY('Ball retainer (plastic)',
'Ball retainer (plastic)',(#10983));
#10943=PRODUCT_RELATED_PRODUCT_CATEGORY('Horizontal guide cap',
'Horizontal guide cap',(#10984));
#10944=PRODUCT_RELATED_PRODUCT_CATEGORY('Upper pin sleeve',
'Upper pin sleeve',(#10985));
#10945=PRODUCT_RELATED_PRODUCT_CATEGORY('Pin keeper','Pin keeper',(#10986));
#10946=PRODUCT_RELATED_PRODUCT_CATEGORY('M4x10 Cap Screw',
'M4x10 Cap Screw',(#10987));
#10947=APPLICATION_PROTOCOL_DEFINITION('international standard',
'automotive_design',2009,#10948);
#10948=APPLICATION_CONTEXT(
'Core Data for Automotive Mechanical Design Process');
#10949=PRODUCT_CONTEXT('part definition',#10948,'mechanical');
#10950=PRODUCT('PAT-096','PAT-096',
'PAT-096',(#10949));
#10951=PRODUCT('Base and guide','Base and guide','Base and guide',(#10949));
#10952=PRODUCT('Demonstrator base','Demonstrator base',
'Demonstrator base',(#10949));
#10953=PRODUCT('M5x14 Cap Screw','M5x14 Cap Screw','M5x14 Cap Screw',(#10949));
#10954=PRODUCT('Pivot pedestal','Pivot pedestal','Pivot pedestal',(#10949));
#10955=PRODUCT('Pivot cap','Pivot cap','Pivot cap',(#10949));
#10956=PRODUCT('Sealed Ball Bearing - 10 x 30 x 9 mm',
'Sealed Ball Bearing - 10 x 30 x 9 mm',
'Sealed Ball Bearing - 10 x 30 x 9 mm',(#10949));
#10957=PRODUCT('Inner ring','Inner ring','Inner ring',(#10949));
#10958=PRODUCT('Outer ring','Outer ring','Outer ring',(#10949));
#10959=PRODUCT('Balls','Balls','Balls',(#10949));
#10960=PRODUCT('Cage','Cage','Cage',(#10949));
#10961=PRODUCT('Seals 2RS','Seals 2RS','Seals 2RS',(#10949));
#10962=PRODUCT('Eighty millimetre guide shaft',
'Eighty millimetre guide shaft','Eighty millimetre guide shaft',(#10949));
#10963=PRODUCT('Horizontal shaft support','Horizontal shaft support',
'Horizontal shaft support',(#10949));
#10964=PRODUCT('Socket Set Screw - M4x6','Socket Set Screw - M4x6',
'Socket Set Screw - M4x6',(#10949));
#10965=PRODUCT('Bell crank','Bell crank','Bell crank',(#10949));
#10966=PRODUCT('Bell crank and spindle','Bell crank and spindle',
'Bell crank and spindle',(#10949));
#10967=PRODUCT('Input grip','Input grip','Input grip',(#10949));
#10968=PRODUCT('Lower race sleeve','Lower race sleeve',
'Lower race sleeve',(#10949));
#10969=PRODUCT('Spindle collar','Spindle collar','Spindle collar',(#10949));
#10970=PRODUCT('Cap Screw - M4x16','Cap Screw - M4x16',
'Cap Screw - M4x16',(#10949));
#10971=PRODUCT('M4x4 collar screw','M4x4 collar screw',
'M4x4 collar screw',(#10949));
#10972=PRODUCT('Horizontal link pin','Horizontal link pin',
'Horizontal link pin',(#10949));
#10973=PRODUCT('Horizontal lower pin sleeve',
'Horizontal lower pin sleeve','Horizontal lower pin sleeve',(#10949));
#10974=PRODUCT('Connecting link','Connecting link','Connecting link',(#10949));
#10975=PRODUCT('Offset connecting link','Offset connecting link',
'Offset connecting link',(#10949));
#10976=PRODUCT('Plain link bushing','Plain link bushing',
'Plain link bushing',(#10949));
#10977=PRODUCT('Output slider','Output slider','Output slider',(#10949));
#10978=PRODUCT('Carriage link pin','Carriage link pin',
'Carriage link pin',(#10949));
#10979=PRODUCT('Carriage pin sleeve','Carriage pin sleeve',
'Carriage pin sleeve',(#10949));
#10980=PRODUCT('Horizontal output housing','Horizontal output housing',
'Horizontal output housing',(#10949));
#10981=PRODUCT('Linear Ball Bushing - 12 x 21 x 30 mm',
'Linear Ball Bushing - 12 x 21 x 30 mm',
'Linear Ball Bushing - 12 x 21 x 30 mm',(#10949));
#10982=PRODUCT('Steel sleeve','Steel sleeve','Steel sleeve',(#10949));
#10983=PRODUCT('Ball retainer (plastic)','Ball retainer (plastic)',
'Ball retainer (plastic)',(#10949));
#10984=PRODUCT('Horizontal guide cap','Horizontal guide cap',
'Horizontal guide cap',(#10949));
#10985=PRODUCT('Upper pin sleeve','Upper pin sleeve','Upper pin sleeve',
(#10949));
#10986=PRODUCT('Pin keeper','Pin keeper','Pin keeper',(#10949));
#10987=PRODUCT('M4x10 Cap Screw','M4x10 Cap Screw','M4x10 Cap Screw',(#10949));
#10988=PRESENTATION_STYLE_ASSIGNMENT((#10995));
#10989=PRESENTATION_STYLE_ASSIGNMENT((#10996));
#10990=PRESENTATION_STYLE_ASSIGNMENT((#10997));
#10991=PRESENTATION_STYLE_ASSIGNMENT((#10998));
#10992=PRESENTATION_STYLE_ASSIGNMENT((#10999));
#10993=PRESENTATION_STYLE_ASSIGNMENT((#11000));
#10994=PRESENTATION_STYLE_ASSIGNMENT((#11001));
#10995=SURFACE_STYLE_USAGE(.BOTH.,#11002);
#10996=SURFACE_STYLE_USAGE(.BOTH.,#11003);
#10997=SURFACE_STYLE_USAGE(.BOTH.,#11004);
#10998=SURFACE_STYLE_USAGE(.BOTH.,#11005);
#10999=SURFACE_STYLE_USAGE(.BOTH.,#11006);
#11000=SURFACE_STYLE_USAGE(.BOTH.,#11007);
#11001=SURFACE_STYLE_USAGE(.BOTH.,#11008);
#11002=SURFACE_SIDE_STYLE('',(#11009));
#11003=SURFACE_SIDE_STYLE('',(#11010));
#11004=SURFACE_SIDE_STYLE('',(#11011));
#11005=SURFACE_SIDE_STYLE('',(#11012));
#11006=SURFACE_SIDE_STYLE('',(#11013));
#11007=SURFACE_SIDE_STYLE('',(#11014));
#11008=SURFACE_SIDE_STYLE('',(#11015));
#11009=SURFACE_STYLE_FILL_AREA(#11016);
#11010=SURFACE_STYLE_FILL_AREA(#11017);
#11011=SURFACE_STYLE_FILL_AREA(#11018);
#11012=SURFACE_STYLE_FILL_AREA(#11019);
#11013=SURFACE_STYLE_FILL_AREA(#11020);
#11014=SURFACE_STYLE_FILL_AREA(#11021);
#11015=SURFACE_STYLE_FILL_AREA(#11022);
#11016=FILL_AREA_STYLE('Steel - Satin',(#11023));
#11017=FILL_AREA_STYLE('CAD Library Painted - Deep blue',(#11024));
#11018=FILL_AREA_STYLE('CAD Library Painted - Graphite',(#11025));
#11019=FILL_AREA_STYLE('CAD Library Painted - Engineering blue',(#11026));
#11020=FILL_AREA_STYLE('CAD Library Painted - Steel gray',(#11027));
#11021=FILL_AREA_STYLE('CAD Library Painted - Off white',(#11028));
#11022=FILL_AREA_STYLE('CAD Library Painted - Light blue',(#11029));
#11023=FILL_AREA_STYLE_COLOUR('Steel - Satin',#11030);
#11024=FILL_AREA_STYLE_COLOUR('CAD Library Painted - Deep blue',#11031);
#11025=FILL_AREA_STYLE_COLOUR('CAD Library Painted - Graphite',#11032);
#11026=FILL_AREA_STYLE_COLOUR('CAD Library Painted - Engineering blue',
#11033);
#11027=FILL_AREA_STYLE_COLOUR('CAD Library Painted - Steel gray',#11034);
#11028=FILL_AREA_STYLE_COLOUR('CAD Library Painted - Off white',#11035);
#11029=FILL_AREA_STYLE_COLOUR('CAD Library Painted - Light blue',#11036);
#11030=COLOUR_RGB('Steel - Satin',0.627450980392157,0.627450980392157,0.627450980392157);
#11031=COLOUR_RGB('CAD Library Painted - Deep blue',0.0784313725490196,
0.203921568627451,0.349019607843137);
#11032=COLOUR_RGB('CAD Library Painted - Graphite',0.0980392156862745,0.109803921568627,
0.125490196078431);
#11033=COLOUR_RGB('CAD Library Painted - Engineering blue',0.12156862745098,
0.356862745098039,0.6);
#11034=COLOUR_RGB('CAD Library Painted - Steel gray',0.592156862745098,
0.631372549019608,0.67843137254902);
#11035=COLOUR_RGB('CAD Library Painted - Off white',0.909803921568627,0.901960784313726,
0.858823529411765);
#11036=COLOUR_RGB('CAD Library Painted - Light blue',0.286274509803922,
0.552941176470588,0.780392156862745);
#11037=COLOUR_RGB('Dark Blue',0.08,0.2,0.34);
#11038=FILL_AREA_STYLE_COLOUR('',#11037);
#11039=FILL_AREA_STYLE('',(#11038));
#11040=SURFACE_STYLE_FILL_AREA(#11039);
#11041=SURFACE_SIDE_STYLE('',(#11040));
#11042=SURFACE_STYLE_USAGE(.BOTH.,#11041);
#11043=PRESENTATION_STYLE_ASSIGNMENT((#11042));
#11044=COLOUR_RGB('Light Blue',0.38,0.62,0.78);
#11045=FILL_AREA_STYLE_COLOUR('',#11044);
#11046=FILL_AREA_STYLE('',(#11045));
#11047=SURFACE_STYLE_FILL_AREA(#11046);
#11048=SURFACE_SIDE_STYLE('',(#11047));
#11049=SURFACE_STYLE_USAGE(.BOTH.,#11048);
#11050=PRESENTATION_STYLE_ASSIGNMENT((#11049));
#11051=COLOUR_RGB('Sky Blue',0.24,0.69,0.87);
#11052=FILL_AREA_STYLE_COLOUR('',#11051);
#11053=FILL_AREA_STYLE('',(#11052));
#11054=SURFACE_STYLE_FILL_AREA(#11053);
#11055=SURFACE_SIDE_STYLE('',(#11054));
#11056=SURFACE_STYLE_USAGE(.BOTH.,#11055);
#11057=PRESENTATION_STYLE_ASSIGNMENT((#11056));
#11058=COLOUR_RGB('Grey',0.48,0.52,0.57);
#11059=FILL_AREA_STYLE_COLOUR('',#11058);
#11060=FILL_AREA_STYLE('',(#11059));
#11061=SURFACE_STYLE_FILL_AREA(#11060);
#11062=SURFACE_SIDE_STYLE('',(#11061));
#11063=SURFACE_STYLE_USAGE(.BOTH.,#11062);
#11064=PRESENTATION_STYLE_ASSIGNMENT((#11063));
#11065=COLOUR_RGB('Black',0.12,0.14,0.17);
#11066=FILL_AREA_STYLE_COLOUR('',#11065);
#11067=FILL_AREA_STYLE('',(#11066));
#11068=SURFACE_STYLE_FILL_AREA(#11067);
#11069=SURFACE_SIDE_STYLE('',(#11068));
#11070=SURFACE_STYLE_USAGE(.BOTH.,#11069);
#11071=PRESENTATION_STYLE_ASSIGNMENT((#11070));
#11072=COLOUR_RGB('Off White',0.89,0.88,0.83);
#11073=FILL_AREA_STYLE_COLOUR('',#11072);
#11074=FILL_AREA_STYLE('',(#11073));
#11075=SURFACE_STYLE_FILL_AREA(#11074);
#11076=SURFACE_SIDE_STYLE('',(#11075));
#11077=SURFACE_STYLE_USAGE(.BOTH.,#11076);
#11078=PRESENTATION_STYLE_ASSIGNMENT((#11077));
ENDSEC;
END-ISO-10303-21;
